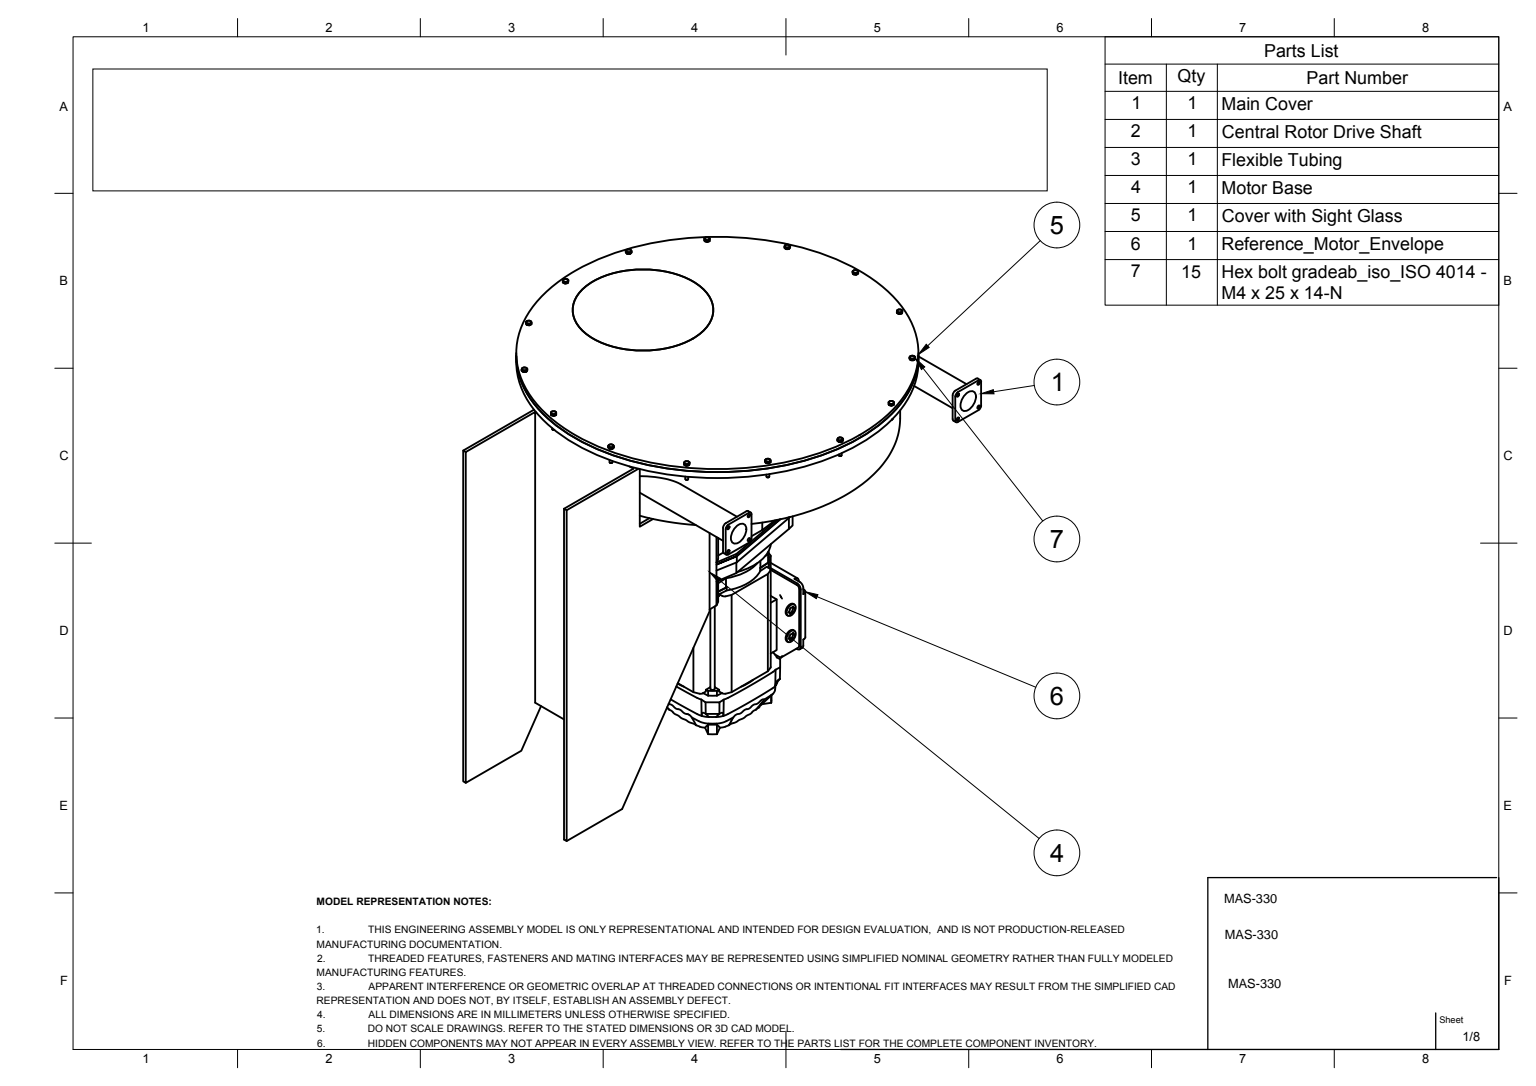
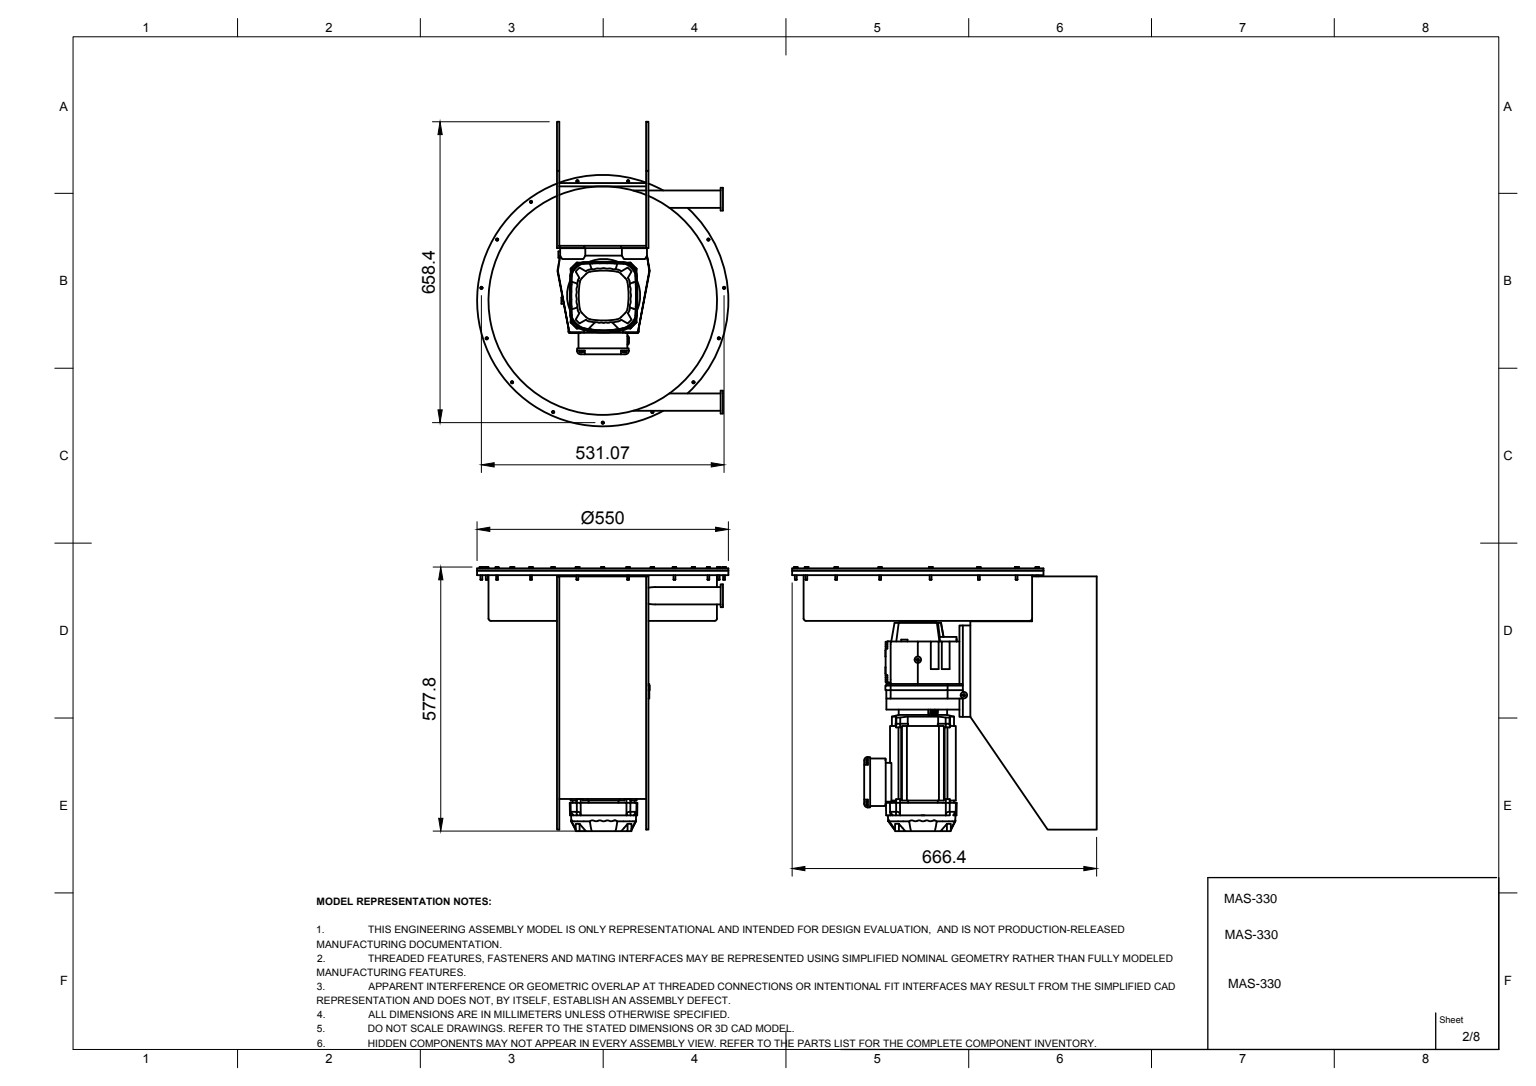
ISO-10303-21;
HEADER;
/* Generated by software containing ST-Developer
 * from STEP Tools, Inc. (www.steptools.com) 
 */

FILE_DESCRIPTION(
/* description */ ('STEP AP214'),
/* implementation_level */ '2;1');

FILE_NAME(
/* name */ 'MAS-330',
/* time_stamp */ '2026-10-12T14:05:15-07:00',
/* author */ (''),
/* organization */ (''),
/* preprocessor_version */ 'ST-DEVELOPER v20.2',
/* originating_system */ 'Autodesk Translation Framework v15.15.0.0',
/* authorisation */ '');

FILE_SCHEMA (('AUTOMOTIVE_DESIGN { 1 0 10303 214 3 1 1 }'));
ENDSEC;

DATA;
#10=MECHANICAL_DESIGN_GEOMETRIC_PRESENTATION_REPRESENTATION('',(#282,#283,
#284,#285,#286,#287,#288,#289),#39959);
#11=ITEM_DEFINED_TRANSFORMATION($,$,#18350,#19989);
#12=ITEM_DEFINED_TRANSFORMATION($,$,#18536,#19990);
#13=ITEM_DEFINED_TRANSFORMATION($,$,#18721,#19991);
#14=ITEM_DEFINED_TRANSFORMATION($,$,#18752,#19992);
#15=ITEM_DEFINED_TRANSFORMATION($,$,#18793,#19993);
#16=ITEM_DEFINED_TRANSFORMATION($,$,#18852,#19994);
#17=ITEM_DEFINED_TRANSFORMATION($,$,#19944,#19995);
#18=ITEM_DEFINED_TRANSFORMATION($,$,#19944,#19996);
#19=ITEM_DEFINED_TRANSFORMATION($,$,#19944,#19997);
#20=ITEM_DEFINED_TRANSFORMATION($,$,#19944,#19998);
#21=ITEM_DEFINED_TRANSFORMATION($,$,#19944,#19999);
#22=ITEM_DEFINED_TRANSFORMATION($,$,#19944,#20000);
#23=ITEM_DEFINED_TRANSFORMATION($,$,#19944,#20001);
#24=ITEM_DEFINED_TRANSFORMATION($,$,#19944,#20002);
#25=ITEM_DEFINED_TRANSFORMATION($,$,#19944,#20003);
#26=ITEM_DEFINED_TRANSFORMATION($,$,#19944,#20004);
#27=ITEM_DEFINED_TRANSFORMATION($,$,#19944,#20005);
#28=ITEM_DEFINED_TRANSFORMATION($,$,#19944,#20006);
#29=ITEM_DEFINED_TRANSFORMATION($,$,#19944,#20007);
#30=ITEM_DEFINED_TRANSFORMATION($,$,#19944,#20008);
#31=ITEM_DEFINED_TRANSFORMATION($,$,#19944,#20009);
#32=(
REPRESENTATION_RELATIONSHIP($,$,#40002,#40001)
REPRESENTATION_RELATIONSHIP_WITH_TRANSFORMATION(#11)
SHAPE_REPRESENTATION_RELATIONSHIP()
);
#33=(
REPRESENTATION_RELATIONSHIP($,$,#40003,#40001)
REPRESENTATION_RELATIONSHIP_WITH_TRANSFORMATION(#12)
SHAPE_REPRESENTATION_RELATIONSHIP()
);
#34=(
REPRESENTATION_RELATIONSHIP($,$,#40004,#40001)
REPRESENTATION_RELATIONSHIP_WITH_TRANSFORMATION(#13)
SHAPE_REPRESENTATION_RELATIONSHIP()
);
#35=(
REPRESENTATION_RELATIONSHIP($,$,#40005,#40001)
REPRESENTATION_RELATIONSHIP_WITH_TRANSFORMATION(#14)
SHAPE_REPRESENTATION_RELATIONSHIP()
);
#36=(
REPRESENTATION_RELATIONSHIP($,$,#40006,#40001)
REPRESENTATION_RELATIONSHIP_WITH_TRANSFORMATION(#15)
SHAPE_REPRESENTATION_RELATIONSHIP()
);
#37=(
REPRESENTATION_RELATIONSHIP($,$,#40007,#40001)
REPRESENTATION_RELATIONSHIP_WITH_TRANSFORMATION(#16)
SHAPE_REPRESENTATION_RELATIONSHIP()
);
#38=(
REPRESENTATION_RELATIONSHIP($,$,#40008,#40001)
REPRESENTATION_RELATIONSHIP_WITH_TRANSFORMATION(#17)
SHAPE_REPRESENTATION_RELATIONSHIP()
);
#39=(
REPRESENTATION_RELATIONSHIP($,$,#40008,#40001)
REPRESENTATION_RELATIONSHIP_WITH_TRANSFORMATION(#18)
SHAPE_REPRESENTATION_RELATIONSHIP()
);
#40=(
REPRESENTATION_RELATIONSHIP($,$,#40008,#40001)
REPRESENTATION_RELATIONSHIP_WITH_TRANSFORMATION(#19)
SHAPE_REPRESENTATION_RELATIONSHIP()
);
#41=(
REPRESENTATION_RELATIONSHIP($,$,#40008,#40001)
REPRESENTATION_RELATIONSHIP_WITH_TRANSFORMATION(#20)
SHAPE_REPRESENTATION_RELATIONSHIP()
);
#42=(
REPRESENTATION_RELATIONSHIP($,$,#40008,#40001)
REPRESENTATION_RELATIONSHIP_WITH_TRANSFORMATION(#21)
SHAPE_REPRESENTATION_RELATIONSHIP()
);
#43=(
REPRESENTATION_RELATIONSHIP($,$,#40008,#40001)
REPRESENTATION_RELATIONSHIP_WITH_TRANSFORMATION(#22)
SHAPE_REPRESENTATION_RELATIONSHIP()
);
#44=(
REPRESENTATION_RELATIONSHIP($,$,#40008,#40001)
REPRESENTATION_RELATIONSHIP_WITH_TRANSFORMATION(#23)
SHAPE_REPRESENTATION_RELATIONSHIP()
);
#45=(
REPRESENTATION_RELATIONSHIP($,$,#40008,#40001)
REPRESENTATION_RELATIONSHIP_WITH_TRANSFORMATION(#24)
SHAPE_REPRESENTATION_RELATIONSHIP()
);
#46=(
REPRESENTATION_RELATIONSHIP($,$,#40008,#40001)
REPRESENTATION_RELATIONSHIP_WITH_TRANSFORMATION(#25)
SHAPE_REPRESENTATION_RELATIONSHIP()
);
#47=(
REPRESENTATION_RELATIONSHIP($,$,#40008,#40001)
REPRESENTATION_RELATIONSHIP_WITH_TRANSFORMATION(#26)
SHAPE_REPRESENTATION_RELATIONSHIP()
);
#48=(
REPRESENTATION_RELATIONSHIP($,$,#40008,#40001)
REPRESENTATION_RELATIONSHIP_WITH_TRANSFORMATION(#27)
SHAPE_REPRESENTATION_RELATIONSHIP()
);
#49=(
REPRESENTATION_RELATIONSHIP($,$,#40008,#40001)
REPRESENTATION_RELATIONSHIP_WITH_TRANSFORMATION(#28)
SHAPE_REPRESENTATION_RELATIONSHIP()
);
#50=(
REPRESENTATION_RELATIONSHIP($,$,#40008,#40001)
REPRESENTATION_RELATIONSHIP_WITH_TRANSFORMATION(#29)
SHAPE_REPRESENTATION_RELATIONSHIP()
);
#51=(
REPRESENTATION_RELATIONSHIP($,$,#40008,#40001)
REPRESENTATION_RELATIONSHIP_WITH_TRANSFORMATION(#30)
SHAPE_REPRESENTATION_RELATIONSHIP()
);
#52=(
REPRESENTATION_RELATIONSHIP($,$,#40008,#40001)
REPRESENTATION_RELATIONSHIP_WITH_TRANSFORMATION(#31)
SHAPE_REPRESENTATION_RELATIONSHIP()
);
#53=CONTEXT_DEPENDENT_SHAPE_REPRESENTATION(#32,#39980);
#54=CONTEXT_DEPENDENT_SHAPE_REPRESENTATION(#33,#39981);
#55=CONTEXT_DEPENDENT_SHAPE_REPRESENTATION(#34,#39982);
#56=CONTEXT_DEPENDENT_SHAPE_REPRESENTATION(#35,#39983);
#57=CONTEXT_DEPENDENT_SHAPE_REPRESENTATION(#36,#39984);
#58=CONTEXT_DEPENDENT_SHAPE_REPRESENTATION(#37,#39985);
#59=CONTEXT_DEPENDENT_SHAPE_REPRESENTATION(#38,#39986);
#60=CONTEXT_DEPENDENT_SHAPE_REPRESENTATION(#39,#39987);
#61=CONTEXT_DEPENDENT_SHAPE_REPRESENTATION(#40,#39988);
#62=CONTEXT_DEPENDENT_SHAPE_REPRESENTATION(#41,#39989);
#63=CONTEXT_DEPENDENT_SHAPE_REPRESENTATION(#42,#39990);
#64=CONTEXT_DEPENDENT_SHAPE_REPRESENTATION(#43,#39991);
#65=CONTEXT_DEPENDENT_SHAPE_REPRESENTATION(#44,#39992);
#66=CONTEXT_DEPENDENT_SHAPE_REPRESENTATION(#45,#39993);
#67=CONTEXT_DEPENDENT_SHAPE_REPRESENTATION(#46,#39994);
#68=CONTEXT_DEPENDENT_SHAPE_REPRESENTATION(#47,#39995);
#69=CONTEXT_DEPENDENT_SHAPE_REPRESENTATION(#48,#39996);
#70=CONTEXT_DEPENDENT_SHAPE_REPRESENTATION(#49,#39997);
#71=CONTEXT_DEPENDENT_SHAPE_REPRESENTATION(#50,#39998);
#72=CONTEXT_DEPENDENT_SHAPE_REPRESENTATION(#51,#39999);
#73=CONTEXT_DEPENDENT_SHAPE_REPRESENTATION(#52,#40000);
#74=NEXT_ASSEMBLY_USAGE_OCCURRENCE('Main Cover:1','Main Cover:1',
'Main Cover:1',#40010,#40011,'Main Cover:1');
#75=NEXT_ASSEMBLY_USAGE_OCCURRENCE('Central Rotor Drive Shaft:1',
'Central Rotor Drive Shaft:1','Central Rotor Drive Shaft:1',#40010,#40012,
'Central Rotor Drive Shaft:1');
#76=NEXT_ASSEMBLY_USAGE_OCCURRENCE('Flexible Tubing:1',
'Flexible Tubing:1','Flexible Tubing:1',#40010,#40013,
'Flexible Tubing:1');
#77=NEXT_ASSEMBLY_USAGE_OCCURRENCE('Motor Base:1','Motor Base:1',
'Motor Base:1',#40010,#40014,'Motor Base:1');
#78=NEXT_ASSEMBLY_USAGE_OCCURRENCE('Cover with Sight Glass:1',
'Cover with Sight Glass:1','Cover with Sight Glass:1',#40010,#40015,
'Cover with Sight Glass:1');
#79=NEXT_ASSEMBLY_USAGE_OCCURRENCE('Reference_Motor_Envelope:1',
'Reference_Motor_Envelope:1','Reference_Motor_Envelope:1',#40010,#40016,
'Reference_Motor_Envelope:1');
#80=NEXT_ASSEMBLY_USAGE_OCCURRENCE(
'hex bolt gradeab_iso_ISO 4014 - M4 x 25 x 14-N:1',
'hex bolt gradeab_iso_ISO 4014 - M4 x 25 x 14-N:1',
'hex bolt gradeab_iso_ISO 4014 - M4 x 25 x 14-N:1',#40010,#40017,
'hex bolt gradeab_iso_ISO 4014 - M4 x 25 x 14-N:1');
#81=NEXT_ASSEMBLY_USAGE_OCCURRENCE(
'hex bolt gradeab_iso_ISO 4014 - M4 x 25 x 14-N:2',
'hex bolt gradeab_iso_ISO 4014 - M4 x 25 x 14-N:2',
'hex bolt gradeab_iso_ISO 4014 - M4 x 25 x 14-N:2',#40010,#40017,
'hex bolt gradeab_iso_ISO 4014 - M4 x 25 x 14-N:2');
#82=NEXT_ASSEMBLY_USAGE_OCCURRENCE(
'hex bolt gradeab_iso_ISO 4014 - M4 x 25 x 14-N:3',
'hex bolt gradeab_iso_ISO 4014 - M4 x 25 x 14-N:3',
'hex bolt gradeab_iso_ISO 4014 - M4 x 25 x 14-N:3',#40010,#40017,
'hex bolt gradeab_iso_ISO 4014 - M4 x 25 x 14-N:3');
#83=NEXT_ASSEMBLY_USAGE_OCCURRENCE(
'hex bolt gradeab_iso_ISO 4014 - M4 x 25 x 14-N:4',
'hex bolt gradeab_iso_ISO 4014 - M4 x 25 x 14-N:4',
'hex bolt gradeab_iso_ISO 4014 - M4 x 25 x 14-N:4',#40010,#40017,
'hex bolt gradeab_iso_ISO 4014 - M4 x 25 x 14-N:4');
#84=NEXT_ASSEMBLY_USAGE_OCCURRENCE(
'hex bolt gradeab_iso_ISO 4014 - M4 x 25 x 14-N:5',
'hex bolt gradeab_iso_ISO 4014 - M4 x 25 x 14-N:5',
'hex bolt gradeab_iso_ISO 4014 - M4 x 25 x 14-N:5',#40010,#40017,
'hex bolt gradeab_iso_ISO 4014 - M4 x 25 x 14-N:5');
#85=NEXT_ASSEMBLY_USAGE_OCCURRENCE(
'hex bolt gradeab_iso_ISO 4014 - M4 x 25 x 14-N:6',
'hex bolt gradeab_iso_ISO 4014 - M4 x 25 x 14-N:6',
'hex bolt gradeab_iso_ISO 4014 - M4 x 25 x 14-N:6',#40010,#40017,
'hex bolt gradeab_iso_ISO 4014 - M4 x 25 x 14-N:6');
#86=NEXT_ASSEMBLY_USAGE_OCCURRENCE(
'hex bolt gradeab_iso_ISO 4014 - M4 x 25 x 14-N:7',
'hex bolt gradeab_iso_ISO 4014 - M4 x 25 x 14-N:7',
'hex bolt gradeab_iso_ISO 4014 - M4 x 25 x 14-N:7',#40010,#40017,
'hex bolt gradeab_iso_ISO 4014 - M4 x 25 x 14-N:7');
#87=NEXT_ASSEMBLY_USAGE_OCCURRENCE(
'hex bolt gradeab_iso_ISO 4014 - M4 x 25 x 14-N:8',
'hex bolt gradeab_iso_ISO 4014 - M4 x 25 x 14-N:8',
'hex bolt gradeab_iso_ISO 4014 - M4 x 25 x 14-N:8',#40010,#40017,
'hex bolt gradeab_iso_ISO 4014 - M4 x 25 x 14-N:8');
#88=NEXT_ASSEMBLY_USAGE_OCCURRENCE(
'hex bolt gradeab_iso_ISO 4014 - M4 x 25 x 14-N:9',
'hex bolt gradeab_iso_ISO 4014 - M4 x 25 x 14-N:9',
'hex bolt gradeab_iso_ISO 4014 - M4 x 25 x 14-N:9',#40010,#40017,
'hex bolt gradeab_iso_ISO 4014 - M4 x 25 x 14-N:9');
#89=NEXT_ASSEMBLY_USAGE_OCCURRENCE(
'hex bolt gradeab_iso_ISO 4014 - M4 x 25 x 14-N:10',
'hex bolt gradeab_iso_ISO 4014 - M4 x 25 x 14-N:10',
'hex bolt gradeab_iso_ISO 4014 - M4 x 25 x 14-N:10',#40010,#40017,
'hex bolt gradeab_iso_ISO 4014 - M4 x 25 x 14-N:10');
#90=NEXT_ASSEMBLY_USAGE_OCCURRENCE(
'hex bolt gradeab_iso_ISO 4014 - M4 x 25 x 14-N:11',
'hex bolt gradeab_iso_ISO 4014 - M4 x 25 x 14-N:11',
'hex bolt gradeab_iso_ISO 4014 - M4 x 25 x 14-N:11',#40010,#40017,
'hex bolt gradeab_iso_ISO 4014 - M4 x 25 x 14-N:11');
#91=NEXT_ASSEMBLY_USAGE_OCCURRENCE(
'hex bolt gradeab_iso_ISO 4014 - M4 x 25 x 14-N:12',
'hex bolt gradeab_iso_ISO 4014 - M4 x 25 x 14-N:12',
'hex bolt gradeab_iso_ISO 4014 - M4 x 25 x 14-N:12',#40010,#40017,
'hex bolt gradeab_iso_ISO 4014 - M4 x 25 x 14-N:12');
#92=NEXT_ASSEMBLY_USAGE_OCCURRENCE(
'hex bolt gradeab_iso_ISO 4014 - M4 x 25 x 14-N:13',
'hex bolt gradeab_iso_ISO 4014 - M4 x 25 x 14-N:13',
'hex bolt gradeab_iso_ISO 4014 - M4 x 25 x 14-N:13',#40010,#40017,
'hex bolt gradeab_iso_ISO 4014 - M4 x 25 x 14-N:13');
#93=NEXT_ASSEMBLY_USAGE_OCCURRENCE(
'hex bolt gradeab_iso_ISO 4014 - M4 x 25 x 14-N:14',
'hex bolt gradeab_iso_ISO 4014 - M4 x 25 x 14-N:14',
'hex bolt gradeab_iso_ISO 4014 - M4 x 25 x 14-N:14',#40010,#40017,
'hex bolt gradeab_iso_ISO 4014 - M4 x 25 x 14-N:14');
#94=NEXT_ASSEMBLY_USAGE_OCCURRENCE(
'hex bolt gradeab_iso_ISO 4014 - M4 x 25 x 14-N:15',
'hex bolt gradeab_iso_ISO 4014 - M4 x 25 x 14-N:15',
'hex bolt gradeab_iso_ISO 4014 - M4 x 25 x 14-N:15',#40010,#40017,
'hex bolt gradeab_iso_ISO 4014 - M4 x 25 x 14-N:15');
#95=SPHERICAL_SURFACE('',#19264,20.3600000000001);
#96=SPHERICAL_SURFACE('',#19265,20.3600000000002);
#97=(
BOUNDED_CURVE()
B_SPLINE_CURVE(3,(#30732,#30733,#30734,#30735),.UNSPECIFIED.,.F.,.F.)
B_SPLINE_CURVE_WITH_KNOTS((4,4),(-1.,-3.7852598383457E-5),.UNSPECIFIED.)
CURVE()
GEOMETRIC_REPRESENTATION_ITEM()
RATIONAL_B_SPLINE_CURVE((1.,0.978516928803385,0.978516115613319,0.999997560429802))
REPRESENTATION_ITEM('')
);
#98=(
BOUNDED_CURVE()
B_SPLINE_CURVE(3,(#30762,#30763,#30764,#30765),.UNSPECIFIED.,.F.,.F.)
B_SPLINE_CURVE_WITH_KNOTS((4,4),(-1.,0.),.UNSPECIFIED.)
CURVE()
GEOMETRIC_REPRESENTATION_ITEM()
RATIONAL_B_SPLINE_CURVE((1.,0.998672257010864,0.998672257010864,1.))
REPRESENTATION_ITEM('')
);
#99=(
BOUNDED_CURVE()
B_SPLINE_CURVE(2,(#31270,#31271,#31272),.UNSPECIFIED.,.F.,.F.)
B_SPLINE_CURVE_WITH_KNOTS((3,3),(-7.67019091974518,-5.57466309126419),
 .UNSPECIFIED.)
CURVE()
GEOMETRIC_REPRESENTATION_ITEM()
RATIONAL_B_SPLINE_CURVE((1.51474535125471,1.4769886104751,1.42144161629559))
REPRESENTATION_ITEM('')
);
#100=(
BOUNDED_CURVE()
B_SPLINE_CURVE(2,(#31276,#31277,#31278),.UNSPECIFIED.,.F.,.F.)
B_SPLINE_CURVE_WITH_KNOTS((3,3),(-18.6605106590412,-16.5649828305604),
 .UNSPECIFIED.)
CURVE()
GEOMETRIC_REPRESENTATION_ITEM()
RATIONAL_B_SPLINE_CURVE((1.4214416162955,1.476988610475,1.51474535125461))
REPRESENTATION_ITEM('')
);
#101=(
BOUNDED_CURVE()
B_SPLINE_CURVE(2,(#31282,#31283,#31284),.UNSPECIFIED.,.F.,.F.)
B_SPLINE_CURVE_WITH_KNOTS((3,3),(-7.6701909197441,-5.57466309126325),
 .UNSPECIFIED.)
CURVE()
GEOMETRIC_REPRESENTATION_ITEM()
RATIONAL_B_SPLINE_CURVE((1.51474535125461,1.47698861047501,1.4214416162955))
REPRESENTATION_ITEM('')
);
#102=(
BOUNDED_CURVE()
B_SPLINE_CURVE(2,(#31288,#31289,#31290),.UNSPECIFIED.,.F.,.F.)
B_SPLINE_CURVE_WITH_KNOTS((3,3),(-18.660510659043,-16.564982830562),
 .UNSPECIFIED.)
CURVE()
GEOMETRIC_REPRESENTATION_ITEM()
RATIONAL_B_SPLINE_CURVE((1.42144161629558,1.47698861047509,1.5147453512547))
REPRESENTATION_ITEM('')
);
#103=(
BOUNDED_CURVE()
B_SPLINE_CURVE(2,(#31295,#31296,#31297),.UNSPECIFIED.,.F.,.F.)
B_SPLINE_CURVE_WITH_KNOTS((3,3),(0.289788647925159,0.47130189078059),
 .UNSPECIFIED.)
CURVE()
GEOMETRIC_REPRESENTATION_ITEM()
RATIONAL_B_SPLINE_CURVE((1.27594103621743,1.36080572125034,1.44372227312264))
REPRESENTATION_ITEM('')
);
#104=(
BOUNDED_CURVE()
B_SPLINE_CURVE(2,(#31299,#31300,#31301),.UNSPECIFIED.,.F.,.F.)
B_SPLINE_CURVE_WITH_KNOTS((3,3),(4.49748593074956,6.56746087072966),
 .UNSPECIFIED.)
CURVE()
GEOMETRIC_REPRESENTATION_ITEM()
RATIONAL_B_SPLINE_CURVE((1.14470058445899,1.15519608505713,1.14470058445899))
REPRESENTATION_ITEM('')
);
#105=(
BOUNDED_CURVE()
B_SPLINE_CURVE(2,(#31302,#31303,#31304),.UNSPECIFIED.,.F.,.F.)
B_SPLINE_CURVE_WITH_KNOTS((3,3),(0.289788647925165,0.4713018907806),
 .UNSPECIFIED.)
CURVE()
GEOMETRIC_REPRESENTATION_ITEM()
RATIONAL_B_SPLINE_CURVE((1.27594103621742,1.36080572125034,1.44372227312264))
REPRESENTATION_ITEM('')
);
#106=(
BOUNDED_CURVE()
B_SPLINE_CURVE(2,(#31308,#31309,#31310),.UNSPECIFIED.,.F.,.F.)
B_SPLINE_CURVE_WITH_KNOTS((3,3),(16.5649828305673,18.6605106590487),
 .UNSPECIFIED.)
CURVE()
GEOMETRIC_REPRESENTATION_ITEM()
RATIONAL_B_SPLINE_CURVE((1.514745351255,1.47698861047538,1.42144161629586))
REPRESENTATION_ITEM('')
);
#107=(
BOUNDED_CURVE()
B_SPLINE_CURVE(2,(#31314,#31315,#31316),.UNSPECIFIED.,.F.,.F.)
B_SPLINE_CURVE_WITH_KNOTS((3,3),(5.57466309126757,7.67019091974901),
 .UNSPECIFIED.)
CURVE()
GEOMETRIC_REPRESENTATION_ITEM()
RATIONAL_B_SPLINE_CURVE((1.4214416162959,1.47698861047542,1.51474535125504))
REPRESENTATION_ITEM('')
);
#108=(
BOUNDED_CURVE()
B_SPLINE_CURVE(2,(#31320,#31321,#31322),.UNSPECIFIED.,.F.,.F.)
B_SPLINE_CURVE_WITH_KNOTS((3,3),(16.5649828305679,18.6605106590493),
 .UNSPECIFIED.)
CURVE()
GEOMETRIC_REPRESENTATION_ITEM()
RATIONAL_B_SPLINE_CURVE((1.51474535125504,1.47698861047542,1.4214416162959))
REPRESENTATION_ITEM('')
);
#109=(
BOUNDED_CURVE()
B_SPLINE_CURVE(2,(#31325,#31326,#31327),.UNSPECIFIED.,.F.,.F.)
B_SPLINE_CURVE_WITH_KNOTS((3,3),(5.5746630912673,7.67019091974871),
 .UNSPECIFIED.)
CURVE()
GEOMETRIC_REPRESENTATION_ITEM()
RATIONAL_B_SPLINE_CURVE((1.42144161629587,1.47698861047539,1.514745351255))
REPRESENTATION_ITEM('')
);
#110=(
BOUNDED_CURVE()
B_SPLINE_CURVE(2,(#32616,#32617,#32618),.UNSPECIFIED.,.F.,.F.)
B_SPLINE_CURVE_WITH_KNOTS((3,3),(-33.3299544599618,-31.4526565385171),
 .UNSPECIFIED.)
CURVE()
GEOMETRIC_REPRESENTATION_ITEM()
RATIONAL_B_SPLINE_CURVE((1.20098306198357,1.20314118954088,1.20441859364838))
REPRESENTATION_ITEM('')
);
#111=(
BOUNDED_CURVE()
B_SPLINE_CURVE(3,(#32734,#32735,#32736,#32737),.UNSPECIFIED.,.F.,.F.)
B_SPLINE_CURVE_WITH_KNOTS((4,4),(0.,1.),.UNSPECIFIED.)
CURVE()
GEOMETRIC_REPRESENTATION_ITEM()
RATIONAL_B_SPLINE_CURVE((0.996955268533354,0.975234645152216,0.976249555641098,
1.))
REPRESENTATION_ITEM('')
);
#112=(
BOUNDED_CURVE()
B_SPLINE_CURVE(3,(#32739,#32740,#32741,#32742),.UNSPECIFIED.,.F.,.F.)
B_SPLINE_CURVE_WITH_KNOTS((4,4),(0.,1.),.UNSPECIFIED.)
CURVE()
GEOMETRIC_REPRESENTATION_ITEM()
RATIONAL_B_SPLINE_CURVE((1.,0.976245441159908,0.975234294192269,0.996966559097083))
REPRESENTATION_ITEM('')
);
#113=(
BOUNDED_CURVE()
B_SPLINE_CURVE(2,(#39863,#39864,#39865),.UNSPECIFIED.,.F.,.F.)
B_SPLINE_CURVE_WITH_KNOTS((3,3),(-0.935215532485105,-0.564489106699794),
 .UNSPECIFIED.)
CURVE()
GEOMETRIC_REPRESENTATION_ITEM()
RATIONAL_B_SPLINE_CURVE((1.84128182081917,1.84128182081917,1.70908373393142))
REPRESENTATION_ITEM('')
);
#114=(
BOUNDED_CURVE()
B_SPLINE_CURVE(2,(#39866,#39867,#39868),.UNSPECIFIED.,.F.,.F.)
B_SPLINE_CURVE_WITH_KNOTS((3,3),(-1.30594195827042,-0.935215532485105),
 .UNSPECIFIED.)
CURVE()
GEOMETRIC_REPRESENTATION_ITEM()
RATIONAL_B_SPLINE_CURVE((1.70908373393142,1.84128182081917,1.84128182081917))
REPRESENTATION_ITEM('')
);
#115=(
BOUNDED_CURVE()
B_SPLINE_CURVE(2,(#39871,#39872,#39873),.UNSPECIFIED.,.F.,.F.)
B_SPLINE_CURVE_WITH_KNOTS((3,3),(-0.935215532485106,-0.564489106699797),
 .UNSPECIFIED.)
CURVE()
GEOMETRIC_REPRESENTATION_ITEM()
RATIONAL_B_SPLINE_CURVE((1.84128182081917,1.84128182081917,1.70908373393142))
REPRESENTATION_ITEM('')
);
#116=(
BOUNDED_CURVE()
B_SPLINE_CURVE(2,(#39874,#39875,#39876),.UNSPECIFIED.,.F.,.F.)
B_SPLINE_CURVE_WITH_KNOTS((3,3),(-1.30594195827041,-0.935215532485105),
 .UNSPECIFIED.)
CURVE()
GEOMETRIC_REPRESENTATION_ITEM()
RATIONAL_B_SPLINE_CURVE((1.70908373393142,1.84128182081917,1.84128182081917))
REPRESENTATION_ITEM('')
);
#117=(
BOUNDED_CURVE()
B_SPLINE_CURVE(2,(#39879,#39880,#39881),.UNSPECIFIED.,.F.,.F.)
B_SPLINE_CURVE_WITH_KNOTS((3,3),(-1.30594195827042,-0.935215532485106),
 .UNSPECIFIED.)
CURVE()
GEOMETRIC_REPRESENTATION_ITEM()
RATIONAL_B_SPLINE_CURVE((1.70908373393142,1.84128182081917,1.84128182081917))
REPRESENTATION_ITEM('')
);
#118=(
BOUNDED_CURVE()
B_SPLINE_CURVE(2,(#39882,#39883,#39884),.UNSPECIFIED.,.F.,.F.)
B_SPLINE_CURVE_WITH_KNOTS((3,3),(-0.935215532485105,-0.564489106699797),
 .UNSPECIFIED.)
CURVE()
GEOMETRIC_REPRESENTATION_ITEM()
RATIONAL_B_SPLINE_CURVE((1.84128182081917,1.84128182081917,1.70908373393142))
REPRESENTATION_ITEM('')
);
#119=(
BOUNDED_CURVE()
B_SPLINE_CURVE(2,(#39887,#39888,#39889),.UNSPECIFIED.,.F.,.F.)
B_SPLINE_CURVE_WITH_KNOTS((3,3),(-1.30594195827042,-0.935215532485105),
 .UNSPECIFIED.)
CURVE()
GEOMETRIC_REPRESENTATION_ITEM()
RATIONAL_B_SPLINE_CURVE((1.70908373393142,1.84128182081917,1.84128182081917))
REPRESENTATION_ITEM('')
);
#120=(
BOUNDED_CURVE()
B_SPLINE_CURVE(2,(#39890,#39891,#39892),.UNSPECIFIED.,.F.,.F.)
B_SPLINE_CURVE_WITH_KNOTS((3,3),(-0.935215532485106,-0.564489106699794),
 .UNSPECIFIED.)
CURVE()
GEOMETRIC_REPRESENTATION_ITEM()
RATIONAL_B_SPLINE_CURVE((1.84128182081917,1.84128182081918,1.70908373393142))
REPRESENTATION_ITEM('')
);
#121=(
BOUNDED_CURVE()
B_SPLINE_CURVE(2,(#39895,#39896,#39897),.UNSPECIFIED.,.F.,.F.)
B_SPLINE_CURVE_WITH_KNOTS((3,3),(-0.935215532485105,-0.564489106699796),
 .UNSPECIFIED.)
CURVE()
GEOMETRIC_REPRESENTATION_ITEM()
RATIONAL_B_SPLINE_CURVE((1.84128182081917,1.84128182081917,1.70908373393142))
REPRESENTATION_ITEM('')
);
#122=(
BOUNDED_CURVE()
B_SPLINE_CURVE(2,(#39898,#39899,#39900),.UNSPECIFIED.,.F.,.F.)
B_SPLINE_CURVE_WITH_KNOTS((3,3),(-1.30594195827041,-0.935215532485106),
 .UNSPECIFIED.)
CURVE()
GEOMETRIC_REPRESENTATION_ITEM()
RATIONAL_B_SPLINE_CURVE((1.70908373393142,1.84128182081917,1.84128182081917))
REPRESENTATION_ITEM('')
);
#123=(
BOUNDED_CURVE()
B_SPLINE_CURVE(2,(#39903,#39904,#39905),.UNSPECIFIED.,.F.,.F.)
B_SPLINE_CURVE_WITH_KNOTS((3,3),(-1.3059419582704,-0.935215532485106),
 .UNSPECIFIED.)
CURVE()
GEOMETRIC_REPRESENTATION_ITEM()
RATIONAL_B_SPLINE_CURVE((1.70908373393143,1.84128182081917,1.84128182081918))
REPRESENTATION_ITEM('')
);
#124=(
BOUNDED_CURVE()
B_SPLINE_CURVE(2,(#39906,#39907,#39908),.UNSPECIFIED.,.F.,.F.)
B_SPLINE_CURVE_WITH_KNOTS((3,3),(-0.935215532485106,-0.564489106699775),
 .UNSPECIFIED.)
CURVE()
GEOMETRIC_REPRESENTATION_ITEM()
RATIONAL_B_SPLINE_CURVE((1.84128182081917,1.84128182081917,1.70908373393141))
REPRESENTATION_ITEM('')
);
#125=ORIENTED_CLOSED_SHELL('',*,#18265,.F.);
#126=ORIENTED_CLOSED_SHELL('',*,#18266,.F.);
#127=ORIENTED_CLOSED_SHELL('',*,#18267,.F.);
#128=ORIENTED_CLOSED_SHELL('',*,#18268,.F.);
#129=CONICAL_SURFACE('',#18879,28.6682517601201,1.23062314824616);
#130=CONICAL_SURFACE('',#18880,50.,0.475882249660419);
#131=CONICAL_SURFACE('',#18882,32.793965079916,0.986624506004945);
#132=CONICAL_SURFACE('',#18883,45.3097394023382,1.52321322351791);
#133=CONICAL_SURFACE('',#18886,0.857142857149273,0.197395559849881);
#134=CONICAL_SURFACE('',#18890,0.999999999925894,0.463647609000806);
#135=CONICAL_SURFACE('',#18893,0.499999999966139,0.463647608692697);
#136=CONICAL_SURFACE('',#18930,107.1412427187,0.174532925199605);
#137=CONICAL_SURFACE('',#18993,76.5,1.3264502315157);
#138=CONICAL_SURFACE('',#19016,6.99999999990287,0.785398163411024);
#139=CONICAL_SURFACE('',#19043,17.4625,0.785398163397448);
#140=CONICAL_SURFACE('',#19069,945.,0.0174532925199452);
#141=CONICAL_SURFACE('',#19072,6.75000000001091,0.785398163397448);
#142=CONICAL_SURFACE('',#19078,942.,0.0174532925199432);
#143=CONICAL_SURFACE('',#19090,6.34999999994079,0.785398163364011);
#144=CONICAL_SURFACE('',#19099,5.4999999998131,1.10714871774448);
#145=CONICAL_SURFACE('',#19291,96.9819619535671,1.14717901504738);
#146=CONICAL_SURFACE('',#19315,22.3000008196592,0.0174532925199444);
#147=CONICAL_SURFACE('',#19317,86.00000081803,0.0174532925199416);
#148=CONICAL_SURFACE('',#19319,22.3000010500621,0.0174532925199414);
#149=CONICAL_SURFACE('',#19321,942.000001054498,0.0174532925199525);
#150=CONICAL_SURFACE('',#19323,22.3000013536827,0.0174532925199416);
#151=CONICAL_SURFACE('',#19325,86.0000013640202,0.0174532925199415);
#152=CONICAL_SURFACE('',#19327,22.3000017511903,0.0174532925199381);
#153=CONICAL_SURFACE('',#19329,22.3000017511903,0.0174532925199378);
#154=CONICAL_SURFACE('',#19331,86.0000013640202,0.0174532925199428);
#155=CONICAL_SURFACE('',#19333,32.8000013531573,0.0174532925199434);
#156=CONICAL_SURFACE('',#19335,200.000000812291,0.0174532925199407);
#157=CONICAL_SURFACE('',#19337,32.8000008122913,0.0174532925199388);
#158=CONICAL_SURFACE('',#19339,86.0000008122913,0.0174532925199416);
#159=CONICAL_SURFACE('',#19341,22.3000008122913,0.0174532925199454);
#160=CONICAL_SURFACE('',#19343,941.999999061101,0.017453292519947);
#161=CONICAL_SURFACE('',#19389,25.2657032643209,0.0174532925199449);
#162=CONICAL_SURFACE('',#19394,25.2657032643207,0.0174532925199417);
#163=CONICAL_SURFACE('',#19396,945.,0.0174532925199452);
#164=CONICAL_SURFACE('',#19398,25.2657032643207,0.0174532925199417);
#165=CONICAL_SURFACE('',#19403,25.2657032643145,0.0174532925199406);
#166=CONICAL_SURFACE('',#19405,25.2657032643204,0.0174532925199395);
#167=CONICAL_SURFACE('',#19410,34.9999999991313,0.0174532925199434);
#168=CONICAL_SURFACE('',#19412,180.,0.017453292519941);
#169=CONICAL_SURFACE('',#19414,34.9999999991315,0.0174532925199386);
#170=CONICAL_SURFACE('',#19419,25.2657032643206,0.0174532925199426);
#171=CONICAL_SURFACE('',#19421,945.,0.0174532925199372);
#172=CONICAL_SURFACE('',#19904,107.1412427187,0.174532925199605);
#173=CONICAL_SURFACE('',#19906,107.1412427187,0.174532925199605);
#174=CONICAL_SURFACE('',#19908,107.1412427187,0.174532925199605);
#175=CONICAL_SURFACE('',#19910,107.1412427187,0.174532925199605);
#176=CONICAL_SURFACE('',#19958,1.61,0.785398163397443);
#177=CONICAL_SURFACE('',#19977,3.5,1.0471975511966);
#178=CONICAL_SURFACE('',#19978,3.5,1.0471975511966);
#179=CONICAL_SURFACE('',#19979,3.5,1.0471975511966);
#180=CONICAL_SURFACE('',#19980,3.5,1.0471975511966);
#181=CONICAL_SURFACE('',#19981,3.5,1.0471975511966);
#182=CONICAL_SURFACE('',#19982,3.5,1.0471975511966);
#183=BREP_WITH_VOIDS('Body1',#18269,(#125,#126,#127,#128));
#184=(
BOUNDED_SURFACE()
B_SPLINE_SURFACE(3,2,((#27814,#27815,#27816),(#27817,#27818,#27819),(#27820,
#27821,#27822),(#27823,#27824,#27825),(#27826,#27827,#27828),(#27829,#27830,
#27831),(#27832,#27833,#27834),(#27835,#27836,#27837),(#27838,#27839,#27840),
(#27841,#27842,#27843),(#27844,#27845,#27846),(#27847,#27848,#27849),(#27850,
#27851,#27852),(#27853,#27854,#27855),(#27856,#27857,#27858),(#27859,#27860,
#27861),(#27862,#27863,#27864),(#27865,#27866,#27867),(#27868,#27869,#27870),
(#27871,#27872,#27873),(#27874,#27875,#27876),(#27877,#27878,#27879),(#27880,
#27881,#27882),(#27883,#27884,#27885),(#27886,#27887,#27888),(#27889,#27890,
#27891),(#27892,#27893,#27894),(#27895,#27896,#27897),(#27898,#27899,#27900),
(#27901,#27902,#27903),(#27904,#27905,#27906),(#27907,#27908,#27909),(#27910,
#27911,#27912),(#27913,#27914,#27915),(#27916,#27917,#27918),(#27919,#27920,
#27921),(#27922,#27923,#27924),(#27925,#27926,#27927),(#27928,#27929,#27930),
(#27931,#27932,#27933),(#27934,#27935,#27936),(#27937,#27938,#27939),(#27940,
#27941,#27942),(#27943,#27944,#27945),(#27946,#27947,#27948),(#27949,#27950,
#27951),(#27952,#27953,#27954),(#27955,#27956,#27957),(#27958,#27959,#27960),
(#27961,#27962,#27963),(#27964,#27965,#27966),(#27967,#27968,#27969),(#27970,
#27971,#27972),(#27973,#27974,#27975),(#27976,#27977,#27978),(#27979,#27980,
#27981),(#27982,#27983,#27984),(#27985,#27986,#27987),(#27988,#27989,#27990),
(#27991,#27992,#27993),(#27994,#27995,#27996),(#27997,#27998,#27999),(#28000,
#28001,#28002),(#28003,#28004,#28005),(#28006,#28007,#28008),(#28009,#28010,
#28011),(#28012,#28013,#28014),(#28015,#28016,#28017),(#28018,#28019,#28020),
(#28021,#28022,#28023),(#28024,#28025,#28026),(#28027,#28028,#28029),(#28030,
#28031,#28032),(#28033,#28034,#28035),(#28036,#28037,#28038),(#28039,#28040,
#28041),(#28042,#28043,#28044),(#28045,#28046,#28047),(#28048,#28049,#28050),
(#28051,#28052,#28053),(#28054,#28055,#28056),(#28057,#28058,#28059),(#28060,
#28061,#28062),(#28063,#28064,#28065),(#28066,#28067,#28068),(#28069,#28070,
#28071),(#28072,#28073,#28074),(#28075,#28076,#28077),(#28078,#28079,#28080),
(#28081,#28082,#28083),(#28084,#28085,#28086),(#28087,#28088,#28089),(#28090,
#28091,#28092),(#28093,#28094,#28095),(#28096,#28097,#28098),(#28099,#28100,
#28101)),.UNSPECIFIED.,.F.,.F.,.F.)
B_SPLINE_SURFACE_WITH_KNOTS((4,2,2,2,2,2,2,2,2,2,2,2,2,2,2,2,2,2,2,2,2,
2,2,2,2,2,2,2,2,2,2,2,2,2,2,2,2,2,2,2,2,2,2,2,2,2,2,4),(3,3),(0.22178007142157,
0.223701231496081,0.225435349569694,0.227169467643307,0.228036526680114,
0.228903585716921,0.229770644753727,0.230204174272131,0.230637703790534,
0.231071233308937,0.231504762827341,0.231938292345744,0.232371821864147,
0.232805351382551,0.233238880900954,0.234105939937761,0.234972998974567,
0.235840058011374,0.237574176084987,0.239308294158601,0.241042412232214,
0.242776530305827,0.246244766453054,0.249713002600281,0.256649474894734,
0.260117711041961,0.263585947189187,0.270522419483641,0.277458891778094,
0.291331836367001,0.298268308661454,0.305204780955908,0.319077725544815,
0.332950670133721,0.346823614722628,0.353760087017082,0.360696559311535,
0.374569503900442,0.388442448489349,0.402315393078255,0.409251865372709,
0.416188337667162,0.423124809961615,0.430061282256069,0.433529518403295,
0.436997754550522,0.440465990697749,0.444121268845909),(-0.000187042000933031,
1.00006570533259),.UNSPECIFIED.)
GEOMETRIC_REPRESENTATION_ITEM()
RATIONAL_B_SPLINE_SURFACE(((1.00001671480553,0.955315105954543,1.00000587097346),
(1.00001553678529,0.958464392346589,1.00000545720104),(1.00001436299837,
0.961602361500747,1.00000504491554),(1.00001214511377,0.96753159221984,
1.00000426589711),(1.0000110971902,0.970333081805704,1.00000389782035),
(1.00000903364032,0.975849718381431,1.00000317301105),(1.00000802454064,
0.978547417281528,1.00000281857094),(1.00000657099102,0.982433296228171,
1.0000023080205),(1.0000060954059,0.98370471220148,1.00000214097413),(1.0000051861456,
0.986135503257278,1.000001821602),(1.00000475111726,0.987298495868281,1.00000166880095),
(1.00000393900491,0.989469574341258,1.00000138355144),(1.00000355798186,
0.990488190713896,1.00000124971942),(1.00000307531353,0.991778542734027,
1.00000108018511),(1.00000292909575,0.992169437270804,1.00000102882701),
(1.00000267340501,0.992852993744571,1.0000009390172),(1.00000256420741,
0.993144919550281,1.00000090066221),(1.00000239821197,0.993588687122249,
1.00000084235732),(1.00000234012324,0.993743979916236,1.00000082195401),
(1.00000227962719,0.993905708377709,1.00000080070514),(1.00000227804363,
0.993909941827738,1.00000080014892),(1.00000233322191,0.993762429746366,
1.00000081952996),(1.00000238907502,0.993613113593466,1.00000083914802),
(1.00000255214859,0.993177157271913,1.00000089642662),(1.00000265990449,
0.992889085671756,1.00000093427522),(1.00000291128676,0.992217047317989,
1.00000102257171),(1.00000305564197,0.991831132138118,1.0000010732756),
(1.00000337449658,0.990978715127399,1.00000118527134),(1.00000355003229,
0.990509442879127,1.00000124692718),(1.00000410591494,0.98902336174389,
1.00000144217757),(1.00000451382822,0.987932857764997,1.00000158545462),
(1.0000053771532,0.985624868901155,1.00000188869225),(1.00000583381796,
0.984404034076013,1.00000204909296),(1.00000677789068,0.981880176447102,
1.00000238069275),(1.00000726052111,0.980589925744053,1.00000255021374),
(1.00000873064634,0.976659734042192,1.00000306658626),(1.00000973994235,
0.973961510289341,1.00000342109532),(1.00001179196766,0.968475683150999,
1.00000414185669),(1.00001283513645,0.96568690486921,1.00000450826337),
(1.00001494361968,0.960050144712234,1.00000524885524),(1.00001601138312,
0.95719561576597,1.00000562390063),(1.00001814845983,0.951482414616923,
1.00000637453578),(1.00001921796653,0.948623225275015,1.00000675019349),
(1.00002242616289,0.940046522775516,1.00000787705289),(1.00002456438731,
0.934330253373406,1.00000862809117),(1.00002882929853,0.922928558871327,
1.00001012611521),(1.00003095610456,0.91724281507434,1.00001087314285),
(1.00003730979308,0.900257041725582,1.00001310483718),(1.00004150973089,
0.889029045332982,1.00001458003971),(1.00004772883642,0.872403062390114,
1.00001676446258),(1.00004978850184,0.866896810424999,1.00001748790749),
(1.00005387724354,0.855966082598523,1.00001892405307),(1.00005590801946,
0.850537063013456,1.00001963735072),(1.00006192256307,0.834457950174723,
1.00002174992247),(1.00006583638793,0.823994840153908,1.00002312462957),
(1.00007345352895,0.803631388209101,1.00002580010388),(1.00007715685939,
0.793731008091671,1.0000271008761),(1.00008791765573,0.764963395833388,
1.00003088054016),(1.00009462794849,0.747024286693254,1.00003323748955),
(1.00010382896234,0.722426553366422,1.00003646928952),(1.00010675138937,
0.71461381858396,1.00003749577419),(1.00011227304363,0.699852382375851,
1.00003943522156),(1.00011487430917,0.692898231787275,1.00004034890021),
(1.00012212392104,0.673517321968125,1.00004289528215),(1.00012616942783,
0.662702177158641,1.00004431624172),(1.0001325032316,0.645769563161906,
1.00004654095165),(1.00013478994257,0.639656333948816,1.00004734414493),
(1.0001374601242,0.632517944987879,1.00004828202993),(1.00013784258632,
0.631495481447842,1.00004841636742),(1.00013694003487,0.63390833726827,
1.00004809935173),(1.00013639387768,0.635368418638627,1.00004790751735),
(1.00013481186227,0.63959773443293,1.00004735184409),(1.00013378125052,
0.642352943082953,1.000046989848),(1.00013001435257,0.652423262814007,1.00004566674808),
(1.00012660145365,0.661547211425516,1.00004446798815),(1.00011821711893,
0.683961657570758,1.00004152304174),(1.00011324709426,0.697248382663264,
1.0000397773509),(1.00010199064016,0.727341072498234,1.00003582359008),
(1.00009570502111,0.744144870834123,1.00003361580473),(1.00008544083,0.771584872526209,
1.00003001057023),(1.00008187300066,0.781123007795138,1.00002875739195),
(1.000074536318,0.800736690215974,1.00002618042693),(1.00007076318398,0.810823681264022,
1.00002485513662),(1.000063033788,0.831487232491117,1.00002214023345),(1.0000590774879,
0.84206389463353,1.00002075060717),(1.00005100479812,0.863645197935074,
1.00001791512414),(1.00004688833189,0.874650043707415,1.0000164692405),
(1.00004060950573,0.891435682115803,1.00001426384112),(1.00003849870446,
0.897078639254129,1.00001352243505),(1.00003426394995,0.908399713630422,
1.00001203500336),(1.00003213787031,0.914083515546979,1.00001128823086),
(1.00002787459407,0.925480839114136,1.00000979078109),(1.00002573731916,
0.931194570120134,1.00000904007632),(1.00002134529738,0.94293607843551,
1.00000749740547),(1.00001909036436,0.94896435336469,1.000006705374),(1.00001684310806,
0.954972105552579,1.00000591603894)))
REPRESENTATION_ITEM('')
SURFACE()
);
#185=(
BOUNDED_SURFACE()
B_SPLINE_SURFACE(3,2,((#28385,#28386,#28387),(#28388,#28389,#28390),(#28391,
#28392,#28393),(#28394,#28395,#28396),(#28397,#28398,#28399),(#28400,#28401,
#28402),(#28403,#28404,#28405),(#28406,#28407,#28408),(#28409,#28410,#28411),
(#28412,#28413,#28414),(#28415,#28416,#28417),(#28418,#28419,#28420),(#28421,
#28422,#28423),(#28424,#28425,#28426),(#28427,#28428,#28429),(#28430,#28431,
#28432),(#28433,#28434,#28435),(#28436,#28437,#28438),(#28439,#28440,#28441),
(#28442,#28443,#28444),(#28445,#28446,#28447),(#28448,#28449,#28450),(#28451,
#28452,#28453),(#28454,#28455,#28456),(#28457,#28458,#28459),(#28460,#28461,
#28462),(#28463,#28464,#28465),(#28466,#28467,#28468),(#28469,#28470,#28471),
(#28472,#28473,#28474),(#28475,#28476,#28477),(#28478,#28479,#28480),(#28481,
#28482,#28483),(#28484,#28485,#28486),(#28487,#28488,#28489),(#28490,#28491,
#28492),(#28493,#28494,#28495),(#28496,#28497,#28498),(#28499,#28500,#28501),
(#28502,#28503,#28504),(#28505,#28506,#28507),(#28508,#28509,#28510),(#28511,
#28512,#28513),(#28514,#28515,#28516),(#28517,#28518,#28519),(#28520,#28521,
#28522),(#28523,#28524,#28525),(#28526,#28527,#28528),(#28529,#28530,#28531),
(#28532,#28533,#28534),(#28535,#28536,#28537),(#28538,#28539,#28540),(#28541,
#28542,#28543),(#28544,#28545,#28546),(#28547,#28548,#28549),(#28550,#28551,
#28552),(#28553,#28554,#28555),(#28556,#28557,#28558),(#28559,#28560,#28561),
(#28562,#28563,#28564),(#28565,#28566,#28567),(#28568,#28569,#28570),(#28571,
#28572,#28573),(#28574,#28575,#28576),(#28577,#28578,#28579),(#28580,#28581,
#28582),(#28583,#28584,#28585),(#28586,#28587,#28588),(#28589,#28590,#28591),
(#28592,#28593,#28594),(#28595,#28596,#28597),(#28598,#28599,#28600),(#28601,
#28602,#28603),(#28604,#28605,#28606),(#28607,#28608,#28609),(#28610,#28611,
#28612),(#28613,#28614,#28615),(#28616,#28617,#28618),(#28619,#28620,#28621),
(#28622,#28623,#28624),(#28625,#28626,#28627),(#28628,#28629,#28630),(#28631,
#28632,#28633),(#28634,#28635,#28636),(#28637,#28638,#28639),(#28640,#28641,
#28642),(#28643,#28644,#28645),(#28646,#28647,#28648),(#28649,#28650,#28651),
(#28652,#28653,#28654),(#28655,#28656,#28657),(#28658,#28659,#28660),(#28661,
#28662,#28663),(#28664,#28665,#28666),(#28667,#28668,#28669),(#28670,#28671,
#28672),(#28673,#28674,#28675),(#28676,#28677,#28678),(#28679,#28680,#28681),
(#28682,#28683,#28684),(#28685,#28686,#28687),(#28688,#28689,#28690)),
 .UNSPECIFIED.,.F.,.F.,.F.)
B_SPLINE_SURFACE_WITH_KNOTS((4,2,2,2,2,2,2,2,2,2,2,2,2,2,2,2,2,2,2,2,2,
2,2,2,2,2,2,2,2,2,2,2,2,2,2,2,2,2,2,2,2,2,2,2,2,2,2,2,2,2,4),(3,3),(0.,
0.00173411807361341,0.00346823614722682,0.00520235422084023,0.00606941325764693,
0.00693647229445363,0.00780353133126034,0.00867059036806704,0.00910411988647039,
0.00953764940487375,0.0099711789232771,0.0104047084416805,0.0108382379600838,
0.0112717674784872,0.0117052969968905,0.0121388265152939,0.0130058855521006,
0.0138729445889073,0.0156070626625207,0.0173411807361341,0.0190752988097475,
0.0208094168833609,0.0242776530305877,0.0277458891778145,0.0346823614722682,
0.038150597619495,0.0416188337667218,0.0485553060611754,0.0554917783556291,
0.0693647229445363,0.0832376675334436,0.0867059036806704,0.0901741398278972,
0.0971106121223509,0.110983556711258,0.124856501300165,0.131792973594619,
0.135261209741846,0.138729445889073,0.15260239047798,0.166475335066887,
0.180348279655794,0.183816515803021,0.187284751950248,0.194221224244702,
0.201157696539155,0.208094168833609,0.211562404980836,0.215030641128063,
0.218498877275289,0.222038288720656),(0.,1.00007117529817),
 .UNSPECIFIED.)
GEOMETRIC_REPRESENTATION_ITEM()
RATIONAL_B_SPLINE_SURFACE(((1.,0.954058032824739,1.00000653986642),(1.,
0.956926189621845,1.00000613158259),(1.,0.959774945923169,1.00000572606044),
(1.,0.965414443781637,1.00000492327455),(1.,0.968205662454782,1.00000452594291),
(1.,0.973699562224279,1.000003743883),(1.,0.976403365991766,1.00000335899492),
(1.,0.98034605056057,1.00000279775142),(1.,0.981641163134558,1.00000261339138),
(1.,0.984176833060148,1.00000225243725),(1.,0.985416251002957,1.00000207600537),
(1.,0.987758111159059,1.00000174264018),(1.,0.988874643995945,1.00000158370106),
(1.,0.99087726268354,1.0000012986271),(1.,0.991757284799027,1.00000117335542),
(1.,0.992797059568252,1.00000102534287),(1.,0.993098523876015,1.00000098242924),
(1.,0.993562924435804,1.00000091632155),(1.,0.993726976585977,1.00000089296862),
(1.,0.9939034030842,1.00000086785421),(1.,0.993913510674876,1.00000086641539),
(1.,0.993776600284822,1.00000088590466),(1.,0.993631545571422,1.00000090655329),
(1.,0.993199734841636,1.0000009680218),(1.,0.992914845213595,1.00000100857601),
(1.,0.99224575536465,1.00000110382135),(1.,0.991859782611137,1.0000011587648),
(1.,0.991003776450707,1.00000128061779),(1.,0.990532224611597,1.00000134774347),
(1.,0.989541347388611,1.00000148879544),(1.,0.98901957113283,1.0000015630706),
(1.,0.987391710342441,1.00000179479755),(1.,0.986223928377901,1.00000196103201),
(1.,0.983775371631144,1.00000230958552),(1.,0.982504716794789,1.000002490464),
(1.,0.97863152044244,1.00000304181581),(1.,0.975951927850889,1.00000342325741),
(1.,0.970485088654407,1.00000420146523),(1.,0.967696119306073,1.00000459847668),
(1.,0.962047336054619,1.00000540258435),(1.,0.959183960598246,1.00000581018755),
(1.,0.953462458079452,1.00000662464684),(1.,0.950596652764379,1.00000703259594),
(1.,0.941994603975872,1.00000825710271),(1.,0.936254194204132,1.00000907425347),
(1.,0.924794890941365,1.00001070549212),(1.,0.919075593477731,1.00001151963753),
(1.,0.901978842716718,1.00001395337019),(1.,0.890663248710558,1.00001556415175),
(1.,0.8738935874927,1.00001795132302),(1.,0.868330212597956,1.00001874327276),
(1.,0.857329904873204,1.00002030917312),(1.,0.851890471291245,1.00002108347973),
(1.,0.835762777169572,1.00002337926661),(1.,0.825264842647475,1.00002487365385),
(1.,0.804827719776929,1.00002778289048),(1.,0.794888487743137,1.00002919774608),
(1.,0.765999443480927,1.00003331011876),(1.,0.747972792915185,1.00003587622322),
(1.,0.714994849965956,1.00004057065307),(1.,0.700044230979255,1.00004269888259),
(1.,0.683764200151961,1.00004501635469),(1.,0.680628844586273,1.00004546267443),
(1.,0.674640520726457,1.0000463151159),(1.,0.671783516007252,1.00004672181222),
(1.,0.663635510374337,1.00004788168568),(1.,0.658767677401333,1.00004857462461),
(1.,0.645945349063695,1.0000503998907),(1.,0.639777818633445,1.00005127784233),
(1.,0.632581312956382,1.00005230226921),(1.,0.631555065114158,1.0000524483562),
(1.,0.63399275055746,1.00005210135022),(1.,0.635466148812585,1.0000518916111),
(1.,0.638664401233599,1.00005143633796),(1.,0.639895676582775,1.00005126106518),
(1.,0.642669442581869,1.00005086621794),(1.,0.644213120868507,1.00005064647441),
(1.,0.652691129180967,1.00004943962487),(1.,0.661906311274784,1.00004812783821),
(1.,0.684528677277457,1.00004490753092),(1.,0.697932027791846,1.00004299955598),
(1.,0.728267963131221,1.00003868121749),(1.,0.745198393491031,1.00003627116063),
(1.,0.768222924620666,1.0000329936049),(1.,0.772921247385803,1.00003232479585),
(1.,0.782497618983893,1.00003096159364),(1.,0.787373779802698,1.00003026746924),
(1.,0.802194699878368,1.00002815770243),(1.,0.812351834256105,1.00002671182829),
(1.,0.833145675250053,1.00002375181263),(1.,0.843782502229831,1.00002223765397),
(1.,0.86547121370724,1.00001915025295),(1.,0.876523345831396,1.00001757697535),
(1.,0.893367253742941,1.00001517923502),(1.,0.899026187982997,1.00001437368235),
(1.,0.910424400977938,1.00001275113994),(1.,0.916164825311843,1.00001193398711),
(1.,0.927638312474702,1.00001030072937),(1.,0.933380131170828,1.00000948337806),
(1.,0.944959178856698,1.00000783509371),(1.,0.950796193416408,1.00000700419121),
(1.,0.95659226878001,1.00000617911642)))
REPRESENTATION_ITEM('')
SURFACE()
);
#186=(
BOUNDED_SURFACE()
B_SPLINE_SURFACE(3,2,((#29356,#29357,#29358),(#29359,#29360,#29361),(#29362,
#29363,#29364),(#29365,#29366,#29367),(#29368,#29369,#29370),(#29371,#29372,
#29373),(#29374,#29375,#29376),(#29377,#29378,#29379),(#29380,#29381,#29382),
(#29383,#29384,#29385),(#29386,#29387,#29388),(#29389,#29390,#29391),(#29392,
#29393,#29394),(#29395,#29396,#29397),(#29398,#29399,#29400),(#29401,#29402,
#29403),(#29404,#29405,#29406),(#29407,#29408,#29409),(#29410,#29411,#29412),
(#29413,#29414,#29415),(#29416,#29417,#29418),(#29419,#29420,#29421),(#29422,
#29423,#29424),(#29425,#29426,#29427),(#29428,#29429,#29430),(#29431,#29432,
#29433),(#29434,#29435,#29436),(#29437,#29438,#29439),(#29440,#29441,#29442),
(#29443,#29444,#29445),(#29446,#29447,#29448),(#29449,#29450,#29451),(#29452,
#29453,#29454),(#29455,#29456,#29457),(#29458,#29459,#29460),(#29461,#29462,
#29463),(#29464,#29465,#29466),(#29467,#29468,#29469),(#29470,#29471,#29472),
(#29473,#29474,#29475),(#29476,#29477,#29478),(#29479,#29480,#29481),(#29482,
#29483,#29484),(#29485,#29486,#29487),(#29488,#29489,#29490),(#29491,#29492,
#29493),(#29494,#29495,#29496),(#29497,#29498,#29499),(#29500,#29501,#29502),
(#29503,#29504,#29505),(#29506,#29507,#29508),(#29509,#29510,#29511),(#29512,
#29513,#29514),(#29515,#29516,#29517),(#29518,#29519,#29520),(#29521,#29522,
#29523),(#29524,#29525,#29526),(#29527,#29528,#29529),(#29530,#29531,#29532),
(#29533,#29534,#29535),(#29536,#29537,#29538),(#29539,#29540,#29541),(#29542,
#29543,#29544),(#29545,#29546,#29547),(#29548,#29549,#29550),(#29551,#29552,
#29553),(#29554,#29555,#29556),(#29557,#29558,#29559),(#29560,#29561,#29562),
(#29563,#29564,#29565),(#29566,#29567,#29568),(#29569,#29570,#29571),(#29572,
#29573,#29574),(#29575,#29576,#29577),(#29578,#29579,#29580),(#29581,#29582,
#29583),(#29584,#29585,#29586),(#29587,#29588,#29589),(#29590,#29591,#29592),
(#29593,#29594,#29595),(#29596,#29597,#29598),(#29599,#29600,#29601),(#29602,
#29603,#29604),(#29605,#29606,#29607),(#29608,#29609,#29610),(#29611,#29612,
#29613),(#29614,#29615,#29616),(#29617,#29618,#29619),(#29620,#29621,#29622),
(#29623,#29624,#29625),(#29626,#29627,#29628),(#29629,#29630,#29631),(#29632,
#29633,#29634),(#29635,#29636,#29637),(#29638,#29639,#29640),(#29641,#29642,
#29643)),.UNSPECIFIED.,.F.,.F.,.F.)
B_SPLINE_SURFACE_WITH_KNOTS((4,2,2,2,2,2,2,2,2,2,2,2,2,2,2,2,2,2,2,2,2,
2,2,2,2,2,2,2,2,2,2,2,2,2,2,2,2,2,2,2,2,2,2,2,2,2,2,4),(3,3),(0.221817496371262,
0.223701231496101,0.225435349569714,0.227169467643327,0.228036526680134,
0.228903585716941,0.229770644753747,0.23020417427215,0.230637703790554,
0.231071233308957,0.23150476282736,0.231938292345764,0.232371821864167,
0.23280535138257,0.233238880900974,0.23410593993778,0.234972998974587,0.235840058011393,
0.237574176085006,0.23930829415862,0.241042412232233,0.242776530305846,
0.246244766453072,0.249713002600299,0.256649474894752,0.260117711041978,
0.263585947189204,0.270522419483657,0.27745889177811,0.291331836367015,
0.298268308661468,0.305204780955921,0.319077725544826,0.332950670133732,
0.346823614722637,0.35376008701709,0.360696559311543,0.374569503900448,
0.388442448489354,0.402315393078259,0.409251865372712,0.416188337667165,
0.423124809961617,0.43006128225607,0.433529518403296,0.436997754550523,
0.440465990697749,0.44408384389623),(-0.000149617051253964,1.00007479383841),
 .UNSPECIFIED.)
GEOMETRIC_REPRESENTATION_ITEM()
RATIONAL_B_SPLINE_SURFACE(((1.00001331480133,0.955500401761319,1.00000665559565),
(1.00001239101105,0.958587815164465,1.00000619382575),(1.00001147053421,
0.961664154694889,1.00000573371211),(1.0000097146529,0.967532512098177,
1.00000485600949),(1.00000887643813,0.970333922314243,1.00000443701574),
(1.00000722584258,0.975850402594055,1.00000361194172),(1.00000641868232,
0.978548025065446,1.00000320847102),(1.00000525601474,0.982433793918799,
1.00000262729484),(1.00000487560295,0.983705173871199,1.00000243714052),
(1.00000414830239,0.986135896059087,1.00000207358883),(1.00000380033123,
0.98729885572081,1.00000189965042),(1.00000315073751,0.989469872683854,
1.00000157494163),(1.00000284596418,0.990488460197697,1.00000142259628),
(1.00000245988668,0.991778775660097,1.00000122960987),(1.00000234292976,
0.992169659122265,1.00000117114726),(1.00000213840745,0.992853196229914,
1.00000106891383),(1.0000020510623,0.993145113764892,1.0000010252531),(1.0000019182856,
0.993588868764268,1.00000095888275),(1.0000018718215,0.993744157158601,
1.000000935657),(1.00000182343182,0.993905881037986,1.00000091146872),(1.00000182216515,
0.993910114368128,1.00000091083556),(1.00000186630125,0.993762606465926,
1.00000093289762),(1.00000191097712,0.993613294543411,1.0000009552295),
(1.00000204141667,0.993177350573097,1.00000102043159),(1.00000212760863,
0.992889287134443,1.00000106351589),(1.00000232868468,0.992217267820518,
1.00000116402665),(1.00000244415175,0.991831363574199,1.00000122174454),
(1.00000269919769,0.990978970713684,1.00000134923293),(1.00000283960547,
0.990509711760598,1.00000141941779),(1.00000328424576,0.989023672728241,
1.00000164167766),(1.00000361052809,0.987933199644816,1.00000180477459),
(1.00000430108584,0.985625276169944,1.00000214995985),(1.00000466636358,
0.984404475932691,1.0000023325492),(1.00000542150997,0.981880689808502,
1.00000271002002),(1.00000580755716,0.980590475660211,1.00000290299128),
(1.00000698348326,0.976660395306211,1.00000349079492),(1.00000779080056,
0.973962247998255,1.00000389434413),(1.00000943217783,0.968476576281456,
1.00000471481025),(1.00001026658934,0.965687877010012,1.00000513190289),
(1.00001195312625,0.960051276550606,1.00000597494271),(1.00001280721057,
0.957196828477568,1.00000640186909),(1.00001451661888,0.951483789191777,
1.00000725634151),(1.00001537209761,0.948624680855099,1.0000076839649),
(1.00001793827481,0.940048221346092,1.00000896670562),(1.00001964860115,
0.934332113895509,1.00000982163693),(1.00002306002512,0.922930742418279,
1.00001152688645),(1.0000247612181,0.917245159708875,1.00001237725232),
(1.00002984341657,0.900259867589174,1.00001491766259),(1.0000332028695,
0.889032189306294,1.00001659693363),(1.00003817741751,0.872406677399274,
1.00001908353327),(1.00003982490596,0.866900581435969,1.00001990705415),
(1.00004309541517,0.855970163292049,1.00002154186539),(1.00004471979543,
0.850541297518764,1.00002235383532),(1.00004953071814,0.834462640227989,
1.00002475864448),(1.00005266131459,0.823999826640663,1.00002632351831),
(1.00005875412544,0.803636951622608,1.00002936909777),(1.00006171635128,
0.79373685199774,1.00003084980912),(1.00007032371416,0.764970054768136,
1.00003515232371),(1.00007569115378,0.747031453875889,1.00003783531589),
(1.00008305087536,0.722434417430132,1.00004151417897),(1.00008538847094,
0.714621904001906,1.00004268265986),(1.00008980514053,0.699860885997467,
1.00004489039591),(1.00009188584494,0.692906932438445,1.00004593046605),
(1.00009768467601,0.673526571699192,1.00004882909547),(1.0001009206024,
0.662711733315835,1.00005044661999),(1.00010598689542,0.645779599024357,
1.0000529790797),(1.00010781599343,0.639666543011674,1.00005389338074),
(1.00010995182255,0.632528356305523,1.00005496100576),(1.00011025774696,
0.631505921714365,1.00005511392649),(1.00010953581267,0.633918709193333,
1.00005475305721),(1.00010909895159,0.635378749188762,1.0000545346859),
(1.00010783352659,0.639607945165404,1.00005390214494),(1.00010700915923,
0.642363075750804,1.00005349007302),(1.00010399608691,0.652433110183563,
1.00005198394532),(1.00010126617189,0.661556800302084,1.00005061935789),
(1.00009455969692,0.683970611397211,1.00004726702956),(1.00009058426569,
0.697256960064698,1.00004527985287),(1.0000815804353,0.727348797329703,
1.00004077915827),(1.00007655268435,0.744152119587061,1.00003826596438),
(1.00006834254686,0.77159134386594,1.00003416200863),(1.00006548870585,
0.781129208903971,1.00003273547501),(1.00005962022847,0.800742335641159,
1.00002980203187),(1.00005660216804,0.810829040908275,1.0000282934108),
(1.0000504195665,0.831492006708402,1.00002520294817),(1.00004725499489,
0.842068369196021,1.00002362109137),(1.00004079779896,0.863649061069833,
1.00002039336876),(1.00003750511341,0.874653595057445,1.00001874747236),
(1.00003248279597,0.891438757903646,1.00001623699448),(1.00003079440489,
0.897081555169982,1.00001539302783),(1.00002740710273,0.908402308800912,
1.00001369983595),(1.00002570649076,0.914085949687904,1.0000128497605),
(1.00002229637459,0.925482950352643,1.00001114516471),(1.00002058680775,
0.931196519480498,1.00001029061304),(1.00001709216721,0.942876010290598,
1.00000854376652),(1.00001530696519,0.948842360878052,1.00000765140752),
(1.00001352770684,0.954788847051718,1.00000676201955)))
REPRESENTATION_ITEM('')
SURFACE()
);
#187=(
BOUNDED_SURFACE()
B_SPLINE_SURFACE(3,2,((#30000,#30001,#30002),(#30003,#30004,#30005),(#30006,
#30007,#30008),(#30009,#30010,#30011),(#30012,#30013,#30014),(#30015,#30016,
#30017),(#30018,#30019,#30020),(#30021,#30022,#30023),(#30024,#30025,#30026),
(#30027,#30028,#30029),(#30030,#30031,#30032),(#30033,#30034,#30035),(#30036,
#30037,#30038),(#30039,#30040,#30041),(#30042,#30043,#30044),(#30045,#30046,
#30047),(#30048,#30049,#30050),(#30051,#30052,#30053),(#30054,#30055,#30056),
(#30057,#30058,#30059),(#30060,#30061,#30062),(#30063,#30064,#30065),(#30066,
#30067,#30068),(#30069,#30070,#30071),(#30072,#30073,#30074),(#30075,#30076,
#30077),(#30078,#30079,#30080),(#30081,#30082,#30083),(#30084,#30085,#30086),
(#30087,#30088,#30089),(#30090,#30091,#30092),(#30093,#30094,#30095),(#30096,
#30097,#30098),(#30099,#30100,#30101),(#30102,#30103,#30104),(#30105,#30106,
#30107),(#30108,#30109,#30110),(#30111,#30112,#30113),(#30114,#30115,#30116),
(#30117,#30118,#30119),(#30120,#30121,#30122),(#30123,#30124,#30125),(#30126,
#30127,#30128),(#30129,#30130,#30131),(#30132,#30133,#30134),(#30135,#30136,
#30137),(#30138,#30139,#30140),(#30141,#30142,#30143),(#30144,#30145,#30146),
(#30147,#30148,#30149),(#30150,#30151,#30152),(#30153,#30154,#30155),(#30156,
#30157,#30158),(#30159,#30160,#30161),(#30162,#30163,#30164),(#30165,#30166,
#30167),(#30168,#30169,#30170),(#30171,#30172,#30173),(#30174,#30175,#30176),
(#30177,#30178,#30179),(#30180,#30181,#30182),(#30183,#30184,#30185),(#30186,
#30187,#30188),(#30189,#30190,#30191),(#30192,#30193,#30194),(#30195,#30196,
#30197),(#30198,#30199,#30200),(#30201,#30202,#30203),(#30204,#30205,#30206),
(#30207,#30208,#30209),(#30210,#30211,#30212),(#30213,#30214,#30215),(#30216,
#30217,#30218),(#30219,#30220,#30221),(#30222,#30223,#30224),(#30225,#30226,
#30227),(#30228,#30229,#30230),(#30231,#30232,#30233),(#30234,#30235,#30236),
(#30237,#30238,#30239),(#30240,#30241,#30242),(#30243,#30244,#30245),(#30246,
#30247,#30248),(#30249,#30250,#30251),(#30252,#30253,#30254),(#30255,#30256,
#30257),(#30258,#30259,#30260),(#30261,#30262,#30263),(#30264,#30265,#30266),
(#30267,#30268,#30269),(#30270,#30271,#30272),(#30273,#30274,#30275),(#30276,
#30277,#30278),(#30279,#30280,#30281),(#30282,#30283,#30284),(#30285,#30286,
#30287),(#30288,#30289,#30290),(#30291,#30292,#30293),(#30294,#30295,#30296),
(#30297,#30298,#30299)),.UNSPECIFIED.,.F.,.F.,.F.)
B_SPLINE_SURFACE_WITH_KNOTS((4,2,2,2,2,2,2,2,2,2,2,2,2,2,2,2,2,2,2,2,2,
2,2,2,2,2,2,2,2,2,2,2,2,2,2,2,2,2,2,2,2,2,2,2,2,2,2,2,2,4),(3,3),(-0.000102234541641357,
0.00346823614722661,0.00520235422083992,0.00606941325764658,0.00693647229445323,
0.00780353133125988,0.00867059036806653,0.00910411988646986,0.00953764940487319,
0.00997117892327651,0.0104047084416798,0.0108382379600832,0.0112717674784865,
0.0117052969968898,0.0121388265152932,0.0130058855520998,0.0138729445889065,
0.0156070626625198,0.0173411807361331,0.0190752988097464,0.0208094168833597,
0.0242776530305863,0.0277458891778129,0.0346823614722661,0.0381505976194928,
0.0416188337667194,0.0485553060611726,0.0554917783556258,0.0693647229445323,
0.0832376675334387,0.0867059036806654,0.090174139827892,0.0971106121223452,
0.110983556711252,0.124856501300158,0.131792973594611,0.135261209741838,
0.138729445889065,0.152602390477971,0.166475335066877,0.180348279655784,
0.183816515803011,0.187284751950237,0.19422122424469,0.201157696539144,
0.208094168833597,0.211562404980823,0.21503064112805,0.218498877275277,
0.22202653747512),(0.,1.00010223454164),.UNSPECIFIED.)
GEOMETRIC_REPRESENTATION_ITEM()
RATIONAL_B_SPLINE_SURFACE(((1.,0.953549407570009,1.00000949771005),(1.,
0.959455865791245,1.00000829002195),(1.,0.965295688977991,1.00000709595866),
(1.,0.973698745410201,1.00000537779342),(1.,0.976402633150356,1.00000482493197),
(1.,0.980345440167197,1.00000401874983),(1.,0.981640592963782,1.00000375393113),
(1.,0.9841763416393,1.00000323544892),(1.,0.985415798074981,1.0000029820184),
(1.,0.987757730962312,1.00000250316553),(1.,0.988874298475363,1.00000227486199),
(1.,0.990876979358417,1.00000186537567),(1.,0.991757028804683,1.00000168543276),
(1.,0.992796835866325,1.00000147282437),(1.,0.993098309536668,1.00000141118232),
(1.,0.99356272451931,1.00000131622382),(1.,0.993726781764482,1.00000128267918),
(1.,0.993903213741988,1.0000012466043),(1.,0.993913321646593,1.00000124453754),
(1.,0.993776407004476,1.00000127253235),(1.,0.993631347786124,1.00000130219248),
(1.,0.993199523645578,1.00000139048717),(1.,0.992914625169687,1.0000014487401),
(1.,0.992245514540845,1.00000158555253),(1.,0.99185952980013,1.00000166447448),
(1.,0.991003497054706,1.00000183950671),(1.,0.990531930570611,1.00000193592748),
(1.,0.989541022573869,1.00000213853753),(1.,0.989019230113308,1.00000224522795),
(1.,0.987391318766343,1.00000257808549),(1.,0.986223500534092,1.00000281686822),
(1.,0.983774867742231,1.00000331753792),(1.,0.982504173443108,1.00000357735562),
(1.,0.978630856801064,1.00000436932912),(1.,0.975951180989188,1.00000491723998),
(1.,0.970484172008772,1.00000603507429),(1.,0.96769511604352,1.00000660535001),
(1.,0.96204615735736,1.00000776038741),(1.,0.959182692973428,1.00000834587735),
(1.,0.953461012761225,1.00000951578406),(1.,0.950595118442744,1.00001010177084),
(1.,0.941992802500896,1.0000118606785),(1.,0.936252214448483,1.00001303445127),
(1.,0.924792555293885,1.00001537759728),(1.,0.919073080205329,1.0000165470531),
(1.,0.901975798471311,1.00002004291863),(1.,0.890659853037534,1.00002235667962),
(1.,0.873889671000668,1.00002578566336),(1.,0.868326123324781,1.00002692323686),
(1.,0.857325473963624,1.00002917252955),(1.,0.851885871450147,1.00003028476009),
(1.,0.83575767644592,1.00003358247733),(1.,0.825259415892199,1.00003572904704),
(1.,0.804821658304747,1.0000399079366),(1.,0.794882117587898,1.00004194026538),
(1.,0.765992176118451,1.00004784736523),(1.,0.74796496570046,1.00005153337242),
(1.,0.714985998549083,1.0000582765516),(1.,0.700034915249734,1.0000613335859),
(1.,0.683754378804637,1.00006466245226),(1.,0.680618925863469,1.00006530355545),
(1.,0.674630416028701,1.00006652802056),(1.,0.671773322578567,1.00006711220784),
(1.,0.663625063888358,1.00006877827483),(1.,0.658757079736063,1.00006977362708),
(1.,0.645934353180302,1.00007239547823),(1.,0.63976663119061,1.00007365658669),
(1.,0.632569902032773,1.0000751280953),(1.,0.631543622312258,1.00007533793778),
(1.,0.633981383455941,1.00007483949099),(1.,0.63545482746786,1.00007453821724),
(1.,0.638653179224426,1.00007388425319),(1.,0.639884492811753,1.00007363248763),
(1.,0.642658344954122,1.00007306532063),(1.,0.644202071179115,1.00007274967634),
(1.,0.652680342816058,1.00007101613191),(1.,0.661895811073965,1.00006913185356),
(1.,0.684518879688121,1.00006450613546),(1.,0.697922646449475,1.00006176547956),
(1.,0.728259523947718,1.00005556252603),(1.,0.745190480114726,1.00005210066894),
(1.,0.768215726310939,1.00004739271796),(1.,0.772914194992678,1.00004643202638),
(1.,0.782490864005998,1.00004447389364),(1.,0.787367176263245,1.00004347683855),
(1.,0.802188556632332,1.00004044632449),(1.,0.81234600646155,1.00003836944003),
(1.,0.833140493248966,1.00003411761038),(1.,0.843777650575237,1.00003194264058),
(1.,0.865467035644792,1.00002750783189),(1.,0.876519511015255,1.00002524794239),
(1.,0.893363942044945,1.00002180377701),(1.,0.899023052036312,1.00002064666398),
(1.,0.910421619025157,1.00001831600944),(1.,0.916162221641087,1.00001714223369),
(1.,0.927636065134229,1.00001479618742),(1.,0.933378062154726,1.00001362212656),
(1.,0.944938051744135,1.00001125846608),(1.,0.950755904868764,1.00001006889499),
(1.,0.956533186645504,1.00000888761948)))
REPRESENTATION_ITEM('')
SURFACE()
);
#188=(
BOUNDED_SURFACE()
B_SPLINE_SURFACE(3,1,((#30722,#30723),(#30724,#30725),(#30726,#30727),(#30728,
#30729)),.UNSPECIFIED.,.F.,.F.,.F.)
B_SPLINE_SURFACE_WITH_KNOTS((4,4),(2,2),(0.,1.),(0.,1.),.UNSPECIFIED.)
GEOMETRIC_REPRESENTATION_ITEM()
RATIONAL_B_SPLINE_SURFACE(((1.,1.),(0.978516115582536,0.975189339715083),
(0.978516115582536,0.975189339715083),(1.,1.)))
REPRESENTATION_ITEM('')
SURFACE()
);
#189=(
BOUNDED_SURFACE()
B_SPLINE_SURFACE(3,1,((#30753,#30754),(#30755,#30756),(#30757,#30758),(#30759,
#30760)),.UNSPECIFIED.,.F.,.F.,.F.)
B_SPLINE_SURFACE_WITH_KNOTS((4,4),(2,2),(0.,1.),(0.,0.740226077012362),
 .UNSPECIFIED.)
GEOMETRIC_REPRESENTATION_ITEM()
RATIONAL_B_SPLINE_SURFACE(((1.,1.),(0.998672257010864,0.999507458473034),
(0.998672257010864,0.999507458473034),(1.,1.)))
REPRESENTATION_ITEM('')
SURFACE()
);
#190=(
BOUNDED_SURFACE()
B_SPLINE_SURFACE(3,1,((#31681,#31682),(#31683,#31684),(#31685,#31686),(#31687,
#31688)),.UNSPECIFIED.,.F.,.F.,.F.)
B_SPLINE_SURFACE_WITH_KNOTS((4,4),(2,2),(0.,1.),(-0.000822310060064629,
0.),.UNSPECIFIED.)
GEOMETRIC_REPRESENTATION_ITEM()
RATIONAL_B_SPLINE_SURFACE(((1.,1.),(0.962057791684876,0.962057791684876),
(0.962057791684876,0.962057791684876),(1.,1.)))
REPRESENTATION_ITEM('')
SURFACE()
);
#191=(
BOUNDED_SURFACE()
B_SPLINE_SURFACE(3,1,((#31700,#31701),(#31702,#31703),(#31704,#31705),(#31706,
#31707)),.UNSPECIFIED.,.F.,.F.,.F.)
B_SPLINE_SURFACE_WITH_KNOTS((4,4),(2,2),(0.,1.),(-0.000910780085741153,
0.),.UNSPECIFIED.)
GEOMETRIC_REPRESENTATION_ITEM()
RATIONAL_B_SPLINE_SURFACE(((1.,1.),(0.962057791684877,0.962057791684877),
(0.962057791684877,0.962057791684877),(1.,1.)))
REPRESENTATION_ITEM('')
SURFACE()
);
#192=(
BOUNDED_SURFACE()
B_SPLINE_SURFACE(3,1,((#31721,#31722),(#31723,#31724),(#31725,#31726),(#31727,
#31728)),.UNSPECIFIED.,.F.,.F.,.F.)
B_SPLINE_SURFACE_WITH_KNOTS((4,4),(2,2),(0.,1.),(0.,1.),.UNSPECIFIED.)
GEOMETRIC_REPRESENTATION_ITEM()
RATIONAL_B_SPLINE_SURFACE(((1.,1.),(0.962057791684877,0.975189339715083),
(0.962057791684877,0.975189339715083),(1.,1.)))
REPRESENTATION_ITEM('')
SURFACE()
);
#193=(
BOUNDED_SURFACE()
B_SPLINE_SURFACE(3,1,((#31772,#31773,#31774),(#31775,#31776,#31777),(#31778,
#31779,#31780),(#31781,#31782,#31783)),.UNSPECIFIED.,.F.,.F.,.F.)
B_SPLINE_SURFACE_WITH_KNOTS((4,4),(2,1,2),(0.633064943864098,0.634076354292062),
(-0.000184246289843766,0.,1.),.UNSPECIFIED.)
GEOMETRIC_REPRESENTATION_ITEM()
RATIONAL_B_SPLINE_SURFACE(((0.791557642220831,0.791557642220831,0.816814678743125),
(0.791557642220831,0.791557642220831,0.816814678743125),(0.791557642220831,
0.791557642220831,0.816814678743125),(0.791557642220831,0.791557642220831,
0.816814678743125)))
REPRESENTATION_ITEM('')
SURFACE()
);
#194=(
BOUNDED_SURFACE()
B_SPLINE_SURFACE(3,1,((#31793,#31794),(#31795,#31796),(#31797,#31798),(#31799,
#31800)),.UNSPECIFIED.,.F.,.F.,.F.)
B_SPLINE_SURFACE_WITH_KNOTS((4,4),(2,2),(0.,0.365923647633872),(0.,1.),
 .UNSPECIFIED.)
GEOMETRIC_REPRESENTATION_ITEM()
RATIONAL_B_SPLINE_SURFACE(((1.,1.),(0.89042205119026,0.903699651216535),
(0.820941265109217,0.84263787732833),(0.791557641756873,0.816814678335385)))
REPRESENTATION_ITEM('')
SURFACE()
);
#195=(
BOUNDED_SURFACE()
B_SPLINE_SURFACE(3,1,((#31831,#31832),(#31833,#31834),(#31835,#31836),(#31837,
#31838)),.UNSPECIFIED.,.F.,.F.,.F.)
B_SPLINE_SURFACE_WITH_KNOTS((4,4),(2,2),(0.,1.),(-0.000981925268428012,
0.),.UNSPECIFIED.)
GEOMETRIC_REPRESENTATION_ITEM()
RATIONAL_B_SPLINE_SURFACE(((1.,1.),(0.96205779168488,0.96205779168488),
(0.96205779168488,0.96205779168488),(1.,1.)))
REPRESENTATION_ITEM('')
SURFACE()
);
#196=(
BOUNDED_SURFACE()
B_SPLINE_SURFACE(3,1,((#31853,#31854),(#31855,#31856),(#31857,#31858),(#31859,
#31860)),.UNSPECIFIED.,.F.,.F.,.F.)
B_SPLINE_SURFACE_WITH_KNOTS((4,4),(2,2),(0.,1.),(0.,1.),.UNSPECIFIED.)
GEOMETRIC_REPRESENTATION_ITEM()
RATIONAL_B_SPLINE_SURFACE(((1.,1.),(0.96205779168488,0.975189339715083),
(0.96205779168488,0.975189339715083),(1.,1.)))
REPRESENTATION_ITEM('')
SURFACE()
);
#197=(
BOUNDED_SURFACE()
B_SPLINE_SURFACE(3,1,((#31906,#31907),(#31908,#31909),(#31910,#31911),(#31912,
#31913)),.UNSPECIFIED.,.F.,.F.,.F.)
B_SPLINE_SURFACE_WITH_KNOTS((4,4),(2,2),(0.,1.),(-0.000863309921543448,
0.),.UNSPECIFIED.)
GEOMETRIC_REPRESENTATION_ITEM()
RATIONAL_B_SPLINE_SURFACE(((1.,1.),(0.96207291357299,0.96207291357299),
(0.96207291357299,0.96207291357299),(1.,1.)))
REPRESENTATION_ITEM('')
SURFACE()
);
#198=(
BOUNDED_SURFACE()
B_SPLINE_SURFACE(3,1,((#31927,#31928),(#31929,#31930),(#31931,#31932),(#31933,
#31934)),.UNSPECIFIED.,.F.,.F.,.F.)
B_SPLINE_SURFACE_WITH_KNOTS((4,4),(2,2),(0.,1.),(0.,1.),.UNSPECIFIED.)
GEOMETRIC_REPRESENTATION_ITEM()
RATIONAL_B_SPLINE_SURFACE(((1.,1.),(0.96207291357299,0.975189339715083),
(0.96207291357299,0.975189339715083),(1.,1.)))
REPRESENTATION_ITEM('')
SURFACE()
);
#199=(
BOUNDED_SURFACE()
B_SPLINE_SURFACE(3,1,((#31980,#31981),(#31982,#31983),(#31984,#31985),(#31986,
#31987)),.UNSPECIFIED.,.F.,.F.,.F.)
B_SPLINE_SURFACE_WITH_KNOTS((4,4),(2,2),(0.,1.),(-0.000880114866331669,
0.),.UNSPECIFIED.)
GEOMETRIC_REPRESENTATION_ITEM()
RATIONAL_B_SPLINE_SURFACE(((1.,1.),(0.962072913572991,0.962072913572991),
(0.962072913572991,0.962072913572991),(1.,1.)))
REPRESENTATION_ITEM('')
SURFACE()
);
#200=(
BOUNDED_SURFACE()
B_SPLINE_SURFACE(3,1,((#32001,#32002),(#32003,#32004),(#32005,#32006),(#32007,
#32008)),.UNSPECIFIED.,.F.,.F.,.F.)
B_SPLINE_SURFACE_WITH_KNOTS((4,4),(2,2),(0.,1.),(-0.000751572727532702,
0.),.UNSPECIFIED.)
GEOMETRIC_REPRESENTATION_ITEM()
RATIONAL_B_SPLINE_SURFACE(((1.,1.),(0.962057791684879,0.962057791684879),
(0.962057791684879,0.962057791684879),(1.,1.)))
REPRESENTATION_ITEM('')
SURFACE()
);
#201=(
BOUNDED_SURFACE()
B_SPLINE_SURFACE(3,1,((#32916,#32917),(#32918,#32919),(#32920,#32921),(#32922,
#32923)),.UNSPECIFIED.,.F.,.F.,.F.)
B_SPLINE_SURFACE_WITH_KNOTS((4,4),(2,2),(0.,1.),(0.,1.),.UNSPECIFIED.)
GEOMETRIC_REPRESENTATION_ITEM()
RATIONAL_B_SPLINE_SURFACE(((1.,1.),(0.962057791684879,0.975189339715082),
(0.962057791684879,0.975189339715082),(1.,1.)))
REPRESENTATION_ITEM('')
SURFACE()
);
#202=(
BOUNDED_SURFACE()
B_SPLINE_SURFACE(3,1,((#32926,#32927,#32928,#32929),(#32930,#32931,#32932,
#32933),(#32934,#32935,#32936,#32937),(#32938,#32939,#32940,#32941),(#32942,
#32943,#32944,#32945),(#32946,#32947,#32948,#32949),(#32950,#32951,#32952,
#32953),(#32954,#32955,#32956,#32957),(#32958,#32959,#32960,#32961),(#32962,
#32963,#32964,#32965)),.UNSPECIFIED.,.F.,.F.,.F.)
B_SPLINE_SURFACE_WITH_KNOTS((4,3,3,4),(2,1,1,2),(-0.000662388520973799,
0.,1.,1.00066238358002),(-0.00076018000588443,0.,0.676109671237994,0.676144257435705),
 .UNSPECIFIED.)
GEOMETRIC_REPRESENTATION_ITEM()
RATIONAL_B_SPLINE_SURFACE(((1.,1.,1.,1.),(1.,1.,1.,1.),(1.,1.,1.,1.),(1.,
1.,1.,1.),(0.998736553042339,0.998736553042339,0.999455940415833,0.999455940415833),
(0.998736553042339,0.998736553042339,0.999455940415833,0.999455940415833),
(1.,1.,1.,1.),(1.,1.,1.,1.),(1.,1.,1.,1.),(1.,1.,1.,1.)))
REPRESENTATION_ITEM('')
SURFACE()
);
#203=(
BOUNDED_SURFACE()
B_SPLINE_SURFACE(3,1,((#32993,#32994),(#32995,#32996),(#32997,#32998),(#32999,
#33000)),.UNSPECIFIED.,.F.,.F.,.F.)
B_SPLINE_SURFACE_WITH_KNOTS((4,4),(2,2),(0.,1.),(0.,1.),.UNSPECIFIED.)
GEOMETRIC_REPRESENTATION_ITEM()
RATIONAL_B_SPLINE_SURFACE(((1.,1.),(0.962072913572991,0.975189339715083),
(0.962072913572991,0.975189339715083),(1.,1.)))
REPRESENTATION_ITEM('')
SURFACE()
);
#204=(
BOUNDED_SURFACE()
B_SPLINE_SURFACE(3,1,((#33002,#33003,#33004,#33005),(#33006,#33007,#33008,
#33009),(#33010,#33011,#33012,#33013),(#33014,#33015,#33016,#33017)),
 .UNSPECIFIED.,.F.,.F.,.F.)
B_SPLINE_SURFACE_WITH_KNOTS((4,4),(2,1,1,2),(0.847974360952231,1.),(-0.000384803530329693,
0.,1.,1.001),.UNSPECIFIED.)
GEOMETRIC_REPRESENTATION_ITEM()
RATIONAL_B_SPLINE_SURFACE(((0.9997286731407,0.9997286731407,0.99414139959028,
0.99414139959028),(0.999802900849163,0.999802900849163,0.995744154600748,
0.995744154600748),(0.999893343135597,0.999893343135597,0.997697021403988,
0.997697021403988),(1.,1.,1.,1.)))
REPRESENTATION_ITEM('')
SURFACE()
);
#205=(
BOUNDED_SURFACE()
B_SPLINE_SURFACE(3,1,((#33043,#33044),(#33045,#33046),(#33047,#33048),(#33049,
#33050)),.UNSPECIFIED.,.F.,.F.,.F.)
B_SPLINE_SURFACE_WITH_KNOTS((4,4),(2,2),(0.,0.366201644461032),(0.,1.),
 .UNSPECIFIED.)
GEOMETRIC_REPRESENTATION_ITEM()
RATIONAL_B_SPLINE_SURFACE(((1.,1.),(0.890338803435454,0.903626490622545),
(0.820835717386409,0.842545118861594),(0.791490741852866,0.816755884717148)))
REPRESENTATION_ITEM('')
SURFACE()
);
#206=(
BOUNDED_SURFACE()
B_SPLINE_SURFACE(3,1,((#33065,#33066),(#33067,#33068),(#33069,#33070),(#33071,
#33072)),.UNSPECIFIED.,.F.,.F.,.F.)
B_SPLINE_SURFACE_WITH_KNOTS((4,4),(2,2),(0.,1.),(0.,0.966511290545803),
 .UNSPECIFIED.)
GEOMETRIC_REPRESENTATION_ITEM()
RATIONAL_B_SPLINE_SURFACE(((1.,1.),(0.969175395688119,0.979164837438946),
(0.969175395688119,0.979164837438946),(1.,1.)))
REPRESENTATION_ITEM('')
SURFACE()
);
#207=(
BOUNDED_SURFACE()
B_SPLINE_SURFACE(3,1,((#33093,#33094),(#33095,#33096),(#33097,#33098),(#33099,
#33100)),.UNSPECIFIED.,.F.,.F.,.F.)
B_SPLINE_SURFACE_WITH_KNOTS((4,4),(2,2),(0.,1.),(0.,1.),.UNSPECIFIED.)
GEOMETRIC_REPRESENTATION_ITEM()
RATIONAL_B_SPLINE_SURFACE(((1.,1.),(0.97852393395982,0.98163056167315),
(0.97852393395982,0.98163056167315),(1.,1.)))
REPRESENTATION_ITEM('')
SURFACE()
);
#208=(
BOUNDED_SURFACE()
B_SPLINE_SURFACE(3,1,((#33115,#33116),(#33117,#33118),(#33119,#33120),(#33121,
#33122)),.UNSPECIFIED.,.F.,.F.,.F.)
B_SPLINE_SURFACE_WITH_KNOTS((4,4),(2,2),(0.,1.),(0.,0.960625757105633),
 .UNSPECIFIED.)
GEOMETRIC_REPRESENTATION_ITEM()
RATIONAL_B_SPLINE_SURFACE(((1.,1.),(0.969713710620478,0.979821031654969),
(0.969713710620478,0.979821031654969),(1.,1.)))
REPRESENTATION_ITEM('')
SURFACE()
);
#209=(
BOUNDED_SURFACE()
B_SPLINE_SURFACE(3,1,((#33145,#33146),(#33147,#33148),(#33149,#33150),(#33151,
#33152)),.UNSPECIFIED.,.F.,.F.,.F.)
B_SPLINE_SURFACE_WITH_KNOTS((4,4),(2,2),(0.,1.),(0.,1.),.UNSPECIFIED.)
GEOMETRIC_REPRESENTATION_ITEM()
RATIONAL_B_SPLINE_SURFACE(((1.,1.),(0.978523933959819,0.981630561673153),
(0.978523933959819,0.981630561673153),(1.,1.)))
REPRESENTATION_ITEM('')
SURFACE()
);
#210=(
BOUNDED_SURFACE()
B_SPLINE_SURFACE(3,1,((#33167,#33168),(#33169,#33170),(#33171,#33172),(#33173,
#33174)),.UNSPECIFIED.,.F.,.F.,.F.)
B_SPLINE_SURFACE_WITH_KNOTS((4,4),(2,2),(0.,1.),(0.,0.966511290545776),
 .UNSPECIFIED.)
GEOMETRIC_REPRESENTATION_ITEM()
RATIONAL_B_SPLINE_SURFACE(((1.,1.),(0.969175395688119,0.979164837438949),
(0.969175395688119,0.979164837438949),(1.,1.)))
REPRESENTATION_ITEM('')
SURFACE()
);
#211=(
BOUNDED_SURFACE()
B_SPLINE_SURFACE(3,1,((#33197,#33198),(#33199,#33200),(#33201,#33202),(#33203,
#33204)),.UNSPECIFIED.,.F.,.F.,.F.)
B_SPLINE_SURFACE_WITH_KNOTS((4,4),(2,2),(0.633798356768784,1.),(0.,1.),
 .UNSPECIFIED.)
GEOMETRIC_REPRESENTATION_ITEM()
RATIONAL_B_SPLINE_SURFACE(((0.791490742148516,0.816755884976974),(0.820835717853236,
0.842545119271855),(0.890338803803731,0.903626490946197),(1.,1.)))
REPRESENTATION_ITEM('')
SURFACE()
);
#212=(
BOUNDED_SURFACE()
B_SPLINE_SURFACE(3,1,((#33226,#33227,#33228,#33229),(#33230,#33231,#33232,
#33233),(#33234,#33235,#33236,#33237),(#33238,#33239,#33240,#33241)),
 .UNSPECIFIED.,.F.,.F.,.F.)
B_SPLINE_SURFACE_WITH_KNOTS((4,4),(2,1,1,2),(0.,0.152025639047805),(-0.000385633117440705,
0.,1.,1.001),.UNSPECIFIED.)
GEOMETRIC_REPRESENTATION_ITEM()
RATIONAL_B_SPLINE_SURFACE(((1.,1.,1.,1.),(0.999893343135597,0.999893343135597,
0.997697021403987,0.997697021403987),(0.999802900849163,0.999802900849163,
0.995744154600747,0.995744154600747),(0.9997286731407,0.9997286731407,0.994141399590279,
0.994141399590279)))
REPRESENTATION_ITEM('')
SURFACE()
);
#213=(
BOUNDED_SURFACE()
B_SPLINE_SURFACE(3,1,((#33248,#33249),(#33250,#33251),(#33252,#33253),(#33254,
#33255)),.UNSPECIFIED.,.F.,.F.,.F.)
B_SPLINE_SURFACE_WITH_KNOTS((4,4),(2,2),(0.,1.),(1.,1.00115361672614),
 .UNSPECIFIED.)
GEOMETRIC_REPRESENTATION_ITEM()
RATIONAL_B_SPLINE_SURFACE(((1.,1.),(0.975189339715083,0.975189339715083),
(0.975189339715083,0.975189339715083),(1.,1.)))
REPRESENTATION_ITEM('')
SURFACE()
);
#214=(
BOUNDED_SURFACE()
B_SPLINE_SURFACE(3,1,((#33256,#33257,#33258,#33259),(#33260,#33261,#33262,
#33263),(#33264,#33265,#33266,#33267),(#33268,#33269,#33270,#33271),(#33272,
#33273,#33274,#33275),(#33276,#33277,#33278,#33279),(#33280,#33281,#33282,
#33283),(#33284,#33285,#33286,#33287),(#33288,#33289,#33290,#33291),(#33292,
#33293,#33294,#33295)),.UNSPECIFIED.,.F.,.F.,.F.)
B_SPLINE_SURFACE_WITH_KNOTS((4,3,3,4),(2,1,1,2),(-0.000651766775030853,
0.,1.,1.00065175575688),(-0.000817120226221179,0.,0.676109671237986,0.676119671237986),
 .UNSPECIFIED.)
GEOMETRIC_REPRESENTATION_ITEM()
RATIONAL_B_SPLINE_SURFACE(((1.,1.,1.,1.),(1.,1.,1.,1.),(1.,1.,1.,1.),(1.,
1.,1.,1.),(0.998736553042339,0.998736553042339,0.999455940415833,0.999455940415833),
(0.998736553042339,0.998736553042339,0.999455940415833,0.999455940415833),
(1.,1.,1.,1.),(1.,1.,1.,1.),(1.,1.,1.,1.),(1.,1.,1.,1.)))
REPRESENTATION_ITEM('')
SURFACE()
);
#215=(
BOUNDED_SURFACE()
B_SPLINE_SURFACE(3,1,((#33318,#33319),(#33320,#33321),(#33322,#33323),(#33324,
#33325)),.UNSPECIFIED.,.F.,.F.,.F.)
B_SPLINE_SURFACE_WITH_KNOTS((4,4),(2,2),(0.,1.),(1.,1.00127139915746),
 .UNSPECIFIED.)
GEOMETRIC_REPRESENTATION_ITEM()
RATIONAL_B_SPLINE_SURFACE(((1.,1.),(0.975189339715083,0.975189339715083),
(0.975189339715083,0.975189339715083),(1.,1.)))
REPRESENTATION_ITEM('')
SURFACE()
);
#216=(
BOUNDED_SURFACE()
B_SPLINE_SURFACE(3,1,((#33333,#33334,#33335,#33336),(#33337,#33338,#33339,
#33340),(#33341,#33342,#33343,#33344),(#33345,#33346,#33347,#33348),(#33349,
#33350,#33351,#33352),(#33353,#33354,#33355,#33356),(#33357,#33358,#33359,
#33360)),.UNSPECIFIED.,.F.,.F.,.F.)
B_SPLINE_SURFACE_WITH_KNOTS((4,3,4),(2,1,1,2),(0.,0.15224442477612,0.152293862972879),
(-0.000531337228447352,0.,1.,1.001),.UNSPECIFIED.)
GEOMETRIC_REPRESENTATION_ITEM()
RATIONAL_B_SPLINE_SURFACE(((1.,1.,1.,1.),(0.999893154836255,0.999893154836255,
0.997693707102185,0.997693707102186),(0.999802576253004,0.999802576253004,
0.995738534439964,0.995738534439964),(0.999728264250248,0.999728264250248,
0.994134482013335,0.994134482013335),(0.999728264250248,0.999728264250248,
0.994134482013335,0.994134482013335),(0.999728264250248,0.999728264250248,
0.994134482013335,0.994134482013335),(0.999728264250248,0.999728264250248,
0.994134482013335,0.994134482013335)))
REPRESENTATION_ITEM('')
SURFACE()
);
#217=(
BOUNDED_SURFACE()
B_SPLINE_SURFACE(3,1,((#33373,#33374,#33375,#33376),(#33377,#33378,#33379,
#33380),(#33381,#33382,#33383,#33384),(#33385,#33386,#33387,#33388)),
 .UNSPECIFIED.,.F.,.F.,.F.)
B_SPLINE_SURFACE_WITH_KNOTS((4,4),(2,1,1,2),(0.847755575223898,1.),(-0.000531332476382396,
0.,1.,1.001),.UNSPECIFIED.)
GEOMETRIC_REPRESENTATION_ITEM()
RATIONAL_B_SPLINE_SURFACE(((0.999728264250248,0.999728264250248,0.994134482013336,
0.994134482013336),(0.999802576253004,0.999802576253004,0.995738534439964,
0.995738534439964),(0.999893154836255,0.999893154836255,0.997693707102186,
0.997693707102186),(1.,1.,1.,1.)))
REPRESENTATION_ITEM('')
SURFACE()
);
#218=(
BOUNDED_SURFACE()
B_SPLINE_SURFACE(3,1,((#33391,#33392,#33393,#33394),(#33395,#33396,#33397,
#33398),(#33399,#33400,#33401,#33402),(#33403,#33404,#33405,#33406)),
 .UNSPECIFIED.,.F.,.F.,.F.)
B_SPLINE_SURFACE_WITH_KNOTS((4,4),(2,1,1,2),(0.365923647633872,0.36753176510902),
(-0.000355481502485282,0.,1.,1.0002958898079),.UNSPECIFIED.)
GEOMETRIC_REPRESENTATION_ITEM()
RATIONAL_B_SPLINE_SURFACE(((0.791557641756873,0.791557641756873,0.816814678335385,
0.816814678335385),(0.791557641756873,0.791557641756873,0.816814678335385,
0.816814678335385),(0.791557641756873,0.791557641756873,0.816814678335385,
0.816814678335385),(0.791557641756873,0.791557641756873,0.816814678335385,
0.816814678335385)))
REPRESENTATION_ITEM('')
SURFACE()
);
#219=(
BOUNDED_SURFACE()
B_SPLINE_SURFACE(3,1,((#33407,#33408),(#33409,#33410),(#33411,#33412),(#33413,
#33414)),.UNSPECIFIED.,.F.,.F.,.F.)
B_SPLINE_SURFACE_WITH_KNOTS((4,4),(2,2),(0.,1.),(0.,0.966044174191949),
 .UNSPECIFIED.)
GEOMETRIC_REPRESENTATION_ITEM()
RATIONAL_B_SPLINE_SURFACE(((1.,1.),(0.969175395688119,0.979160009526791),
(0.969175395688119,0.979160009526791),(1.,1.)))
REPRESENTATION_ITEM('')
SURFACE()
);
#220=(
BOUNDED_SURFACE()
B_SPLINE_SURFACE(3,1,((#33423,#33424),(#33425,#33426),(#33427,#33428),(#33429,
#33430)),.UNSPECIFIED.,.F.,.F.,.F.)
B_SPLINE_SURFACE_WITH_KNOTS((4,4),(2,2),(0.,1.),(0.,1.),.UNSPECIFIED.)
GEOMETRIC_REPRESENTATION_ITEM()
RATIONAL_B_SPLINE_SURFACE(((1.,1.),(0.97852393395982,0.98163056167315),
(0.97852393395982,0.98163056167315),(1.,1.)))
REPRESENTATION_ITEM('')
SURFACE()
);
#221=(
BOUNDED_SURFACE()
B_SPLINE_SURFACE(3,1,((#33432,#33433),(#33434,#33435),(#33436,#33437),(#33438,
#33439)),.UNSPECIFIED.,.F.,.F.,.F.)
B_SPLINE_SURFACE_WITH_KNOTS((4,4),(2,2),(0.,1.),(0.,0.960122375136112),
 .UNSPECIFIED.)
GEOMETRIC_REPRESENTATION_ITEM()
RATIONAL_B_SPLINE_SURFACE(((1.,1.),(0.969713710620478,0.979815735270679),
(0.969713710620478,0.979815735270679),(1.,1.)))
REPRESENTATION_ITEM('')
SURFACE()
);
#222=(
BOUNDED_SURFACE()
B_SPLINE_SURFACE(3,1,((#33448,#33449),(#33450,#33451),(#33452,#33453),(#33454,
#33455)),.UNSPECIFIED.,.F.,.F.,.F.)
B_SPLINE_SURFACE_WITH_KNOTS((4,4),(2,2),(0.,1.),(0.,1.),.UNSPECIFIED.)
GEOMETRIC_REPRESENTATION_ITEM()
RATIONAL_B_SPLINE_SURFACE(((1.,1.),(0.978523933959819,0.981630561673153),
(0.978523933959819,0.981630561673153),(1.,1.)))
REPRESENTATION_ITEM('')
SURFACE()
);
#223=(
BOUNDED_SURFACE()
B_SPLINE_SURFACE(3,1,((#33457,#33458),(#33459,#33460),(#33461,#33462),(#33463,
#33464)),.UNSPECIFIED.,.F.,.F.,.F.)
B_SPLINE_SURFACE_WITH_KNOTS((4,4),(2,2),(0.,1.),(0.,0.966044174191933),
 .UNSPECIFIED.)
GEOMETRIC_REPRESENTATION_ITEM()
RATIONAL_B_SPLINE_SURFACE(((1.,1.),(0.969175395688119,0.979160009526794),
(0.969175395688119,0.979160009526794),(1.,1.)))
REPRESENTATION_ITEM('')
SURFACE()
);
#224=(
BOUNDED_SURFACE()
B_SPLINE_SURFACE(3,1,((#33466,#33467),(#33468,#33469),(#33470,#33471),(#33472,
#33473)),.UNSPECIFIED.,.F.,.F.,.F.)
B_SPLINE_SURFACE_WITH_KNOTS((4,4),(2,2),(0.634076354292062,1.),(0.,1.),
 .UNSPECIFIED.)
GEOMETRIC_REPRESENTATION_ITEM()
RATIONAL_B_SPLINE_SURFACE(((0.791557642220831,0.816814678743125),(0.820941265840603,
0.842637877971094),(0.890422051766993,0.903699651723386),(1.,1.)))
REPRESENTATION_ITEM('')
SURFACE()
);
#225=(
BOUNDED_SURFACE()
B_SPLINE_SURFACE(3,1,((#33474,#33475),(#33476,#33477),(#33478,#33479),(#33480,
#33481)),.UNSPECIFIED.,.F.,.F.,.F.)
B_SPLINE_SURFACE_WITH_KNOTS((4,4),(2,2),(0.,1.),(1.,1.00115971095081),
 .UNSPECIFIED.)
GEOMETRIC_REPRESENTATION_ITEM()
RATIONAL_B_SPLINE_SURFACE(((1.,1.),(0.975189339715083,0.975189339715083),
(0.975189339715083,0.975189339715083),(1.,1.)))
REPRESENTATION_ITEM('')
SURFACE()
);
#226=(
BOUNDED_SURFACE()
B_SPLINE_SURFACE(3,1,((#33482,#33483),(#33484,#33485),(#33486,#33487),(#33488,
#33489),(#33490,#33491),(#33492,#33493),(#33494,#33495),(#33496,#33497),
(#33498,#33499),(#33500,#33501)),.UNSPECIFIED.,.F.,.F.,.F.)
B_SPLINE_SURFACE_WITH_KNOTS((4,3,3,4),(2,2),(-0.000658266375657395,0.,1.,
1.00065830337858),(-0.000823662838273568,0.),.UNSPECIFIED.)
GEOMETRIC_REPRESENTATION_ITEM()
RATIONAL_B_SPLINE_SURFACE(((1.,1.),(1.,1.),(1.,1.),(1.,1.),(0.998672257010864,
0.998672257010864),(0.998672257010864,0.998672257010864),(1.,1.),(1.,1.),
(1.,1.),(1.,1.)))
REPRESENTATION_ITEM('')
SURFACE()
);
#227=(
BOUNDED_SURFACE()
B_SPLINE_SURFACE(3,1,((#33526,#33527),(#33528,#33529),(#33530,#33531),(#33532,
#33533)),.UNSPECIFIED.,.F.,.F.,.F.)
B_SPLINE_SURFACE_WITH_KNOTS((4,4),(2,2),(0.,1.),(-0.000998381213712629,
0.),.UNSPECIFIED.)
GEOMETRIC_REPRESENTATION_ITEM()
RATIONAL_B_SPLINE_SURFACE(((1.,1.),(0.978516115582536,0.978516115582536),
(0.978516115582536,0.978516115582536),(1.,1.)))
REPRESENTATION_ITEM('')
SURFACE()
);
#228=(
BOUNDED_SURFACE()
B_SPLINE_SURFACE(3,1,((#34127,#34128,#34129,#34130),(#34131,#34132,#34133,
#34134),(#34135,#34136,#34137,#34138),(#34139,#34140,#34141,#34142),(#34143,
#34144,#34145,#34146),(#34147,#34148,#34149,#34150),(#34151,#34152,#34153,
#34154),(#34155,#34156,#34157,#34158),(#34159,#34160,#34161,#34162),(#34163,
#34164,#34165,#34166)),.UNSPECIFIED.,.F.,.F.,.F.)
B_SPLINE_SURFACE_WITH_KNOTS((4,3,3,4),(2,1,1,2),(-0.001,0.,0.205321724422313,
0.206321724412313),(-0.000396813100233054,0.,1.,1.001),.UNSPECIFIED.)
GEOMETRIC_REPRESENTATION_ITEM()
RATIONAL_B_SPLINE_SURFACE(((1.,1.,1.,1.),(1.,1.,1.,1.),(1.,1.,1.,1.),(1.,
1.,1.,1.),(0.996948890458759,0.996948890458759,0.996889659273247,0.996889659273247),
(0.994524239989928,0.994524239989928,0.994417939068052,0.994417939068052),
(0.992726048593505,0.992726048593505,0.992584839384415,0.992584839384415),
(0.992726048593505,0.992726048593505,0.992584839384415,0.992584839384415),
(0.992726048593505,0.992726048593505,0.992584839384415,0.992584839384415),
(0.992726048593505,0.992726048593505,0.992584839384415,0.992584839384415)))
REPRESENTATION_ITEM('')
SURFACE()
);
#229=(
BOUNDED_SURFACE()
B_SPLINE_SURFACE(3,1,((#35952,#35953),(#35954,#35955),(#35956,#35957),(#35958,
#35959),(#35960,#35961),(#35962,#35963),(#35964,#35965)),.UNSPECIFIED.,
 .F.,.F.,.F.)
B_SPLINE_SURFACE_WITH_KNOTS((4,3,4),(2,2),(0.,1.,1.00008671004856),(0.,
0.740226077012249),.UNSPECIFIED.)
GEOMETRIC_REPRESENTATION_ITEM()
RATIONAL_B_SPLINE_SURFACE(((1.,1.),(0.998672257010864,0.999507458473034),
(0.998672257010864,0.999507458473034),(1.,1.),(1.,1.),(1.,1.),(1.,1.)))
REPRESENTATION_ITEM('')
SURFACE()
);
#230=(
BOUNDED_SURFACE()
B_SPLINE_SURFACE(3,1,((#35978,#35979),(#35980,#35981),(#35982,#35983),(#35984,
#35985)),.UNSPECIFIED.,.F.,.F.,.F.)
B_SPLINE_SURFACE_WITH_KNOTS((4,4),(2,2),(0.,1.),(0.,1.),.UNSPECIFIED.)
GEOMETRIC_REPRESENTATION_ITEM()
RATIONAL_B_SPLINE_SURFACE(((1.,1.),(0.962057791684876,0.975189339715083),
(0.962057791684876,0.975189339715083),(1.,1.)))
REPRESENTATION_ITEM('')
SURFACE()
);
#231=(
BOUNDED_SURFACE()
B_SPLINE_SURFACE(3,1,((#35998,#35999,#36000,#36001),(#36002,#36003,#36004,
#36005),(#36006,#36007,#36008,#36009),(#36010,#36011,#36012,#36013)),
 .UNSPECIFIED.,.F.,.F.,.F.)
B_SPLINE_SURFACE_WITH_KNOTS((4,4),(2,1,1,2),(0.,0.152244424776119),(-0.000281365801619608,
0.,1.,1.001),.UNSPECIFIED.)
GEOMETRIC_REPRESENTATION_ITEM()
RATIONAL_B_SPLINE_SURFACE(((1.,1.,1.,1.),(0.999893154836255,0.999893154836255,
0.997693707102186,0.997693707102186),(0.999802576253004,0.999802576253004,
0.995738534439964,0.995738534439964),(0.999728264250248,0.999728264250248,
0.994134482013336,0.994134482013336)))
REPRESENTATION_ITEM('')
SURFACE()
);
#232=(
BOUNDED_SURFACE()
B_SPLINE_SURFACE(3,1,((#36027,#36028,#36029,#36030),(#36031,#36032,#36033,
#36034),(#36035,#36036,#36037,#36038),(#36039,#36040,#36041,#36042)),
 .UNSPECIFIED.,.F.,.F.,.F.)
B_SPLINE_SURFACE_WITH_KNOTS((4,4),(2,1,1,2),(0.847755575223896,1.),(-0.000269810410367957,
0.,1.,1.001),.UNSPECIFIED.)
GEOMETRIC_REPRESENTATION_ITEM()
RATIONAL_B_SPLINE_SURFACE(((0.999728264250248,0.999728264250248,0.994134482013336,
0.994134482013336),(0.999802576253004,0.999802576253004,0.995738534439964,
0.995738534439964),(0.999893154836255,0.999893154836255,0.997693707102186,
0.997693707102186),(1.,1.,1.,1.)))
REPRESENTATION_ITEM('')
SURFACE()
);
#233=(
BOUNDED_SURFACE()
B_SPLINE_SURFACE(3,1,((#36063,#36064),(#36065,#36066),(#36067,#36068),(#36069,
#36070)),.UNSPECIFIED.,.F.,.F.,.F.)
B_SPLINE_SURFACE_WITH_KNOTS((4,4),(2,2),(0.,0.365923648059291),(0.,1.),
 .UNSPECIFIED.)
GEOMETRIC_REPRESENTATION_ITEM()
RATIONAL_B_SPLINE_SURFACE(((1.,1.),(0.890422051062866,0.903699651104578),
(0.820941264947662,0.842637877186351),(0.79155764165439,0.816814678245319)))
REPRESENTATION_ITEM('')
SURFACE()
);
#234=(
BOUNDED_SURFACE()
B_SPLINE_SURFACE(3,1,((#36085,#36086),(#36087,#36088),(#36089,#36090),(#36091,
#36092)),.UNSPECIFIED.,.F.,.F.,.F.)
B_SPLINE_SURFACE_WITH_KNOTS((4,4),(2,2),(0.,1.),(0.,0.966044174191948),
 .UNSPECIFIED.)
GEOMETRIC_REPRESENTATION_ITEM()
RATIONAL_B_SPLINE_SURFACE(((1.,1.),(0.969175395688119,0.979160009526791),
(0.969175395688119,0.979160009526791),(1.,1.)))
REPRESENTATION_ITEM('')
SURFACE()
);
#235=(
BOUNDED_SURFACE()
B_SPLINE_SURFACE(3,1,((#36115,#36116),(#36117,#36118),(#36119,#36120),(#36121,
#36122)),.UNSPECIFIED.,.F.,.F.,.F.)
B_SPLINE_SURFACE_WITH_KNOTS((4,4),(2,2),(0.,1.),(0.,1.),.UNSPECIFIED.)
GEOMETRIC_REPRESENTATION_ITEM()
RATIONAL_B_SPLINE_SURFACE(((1.,1.),(0.97852393395982,0.98163056167315),
(0.97852393395982,0.98163056167315),(1.,1.)))
REPRESENTATION_ITEM('')
SURFACE()
);
#236=(
BOUNDED_SURFACE()
B_SPLINE_SURFACE(3,1,((#36137,#36138),(#36139,#36140),(#36141,#36142),(#36143,
#36144)),.UNSPECIFIED.,.F.,.F.,.F.)
B_SPLINE_SURFACE_WITH_KNOTS((4,4),(2,2),(0.,1.),(0.,0.960122375136112),
 .UNSPECIFIED.)
GEOMETRIC_REPRESENTATION_ITEM()
RATIONAL_B_SPLINE_SURFACE(((1.,1.),(0.969713710620478,0.979815735270679),
(0.969713710620478,0.979815735270679),(1.,1.)))
REPRESENTATION_ITEM('')
SURFACE()
);
#237=(
BOUNDED_SURFACE()
B_SPLINE_SURFACE(3,1,((#36167,#36168),(#36169,#36170),(#36171,#36172),(#36173,
#36174)),.UNSPECIFIED.,.F.,.F.,.F.)
B_SPLINE_SURFACE_WITH_KNOTS((4,4),(2,2),(0.,1.),(0.,1.),.UNSPECIFIED.)
GEOMETRIC_REPRESENTATION_ITEM()
RATIONAL_B_SPLINE_SURFACE(((1.,1.),(0.978523933959819,0.981630561673153),
(0.978523933959819,0.981630561673153),(1.,1.)))
REPRESENTATION_ITEM('')
SURFACE()
);
#238=(
BOUNDED_SURFACE()
B_SPLINE_SURFACE(3,1,((#36189,#36190),(#36191,#36192),(#36193,#36194),(#36195,
#36196)),.UNSPECIFIED.,.F.,.F.,.F.)
B_SPLINE_SURFACE_WITH_KNOTS((4,4),(2,2),(0.,1.),(0.,0.966044174191938),
 .UNSPECIFIED.)
GEOMETRIC_REPRESENTATION_ITEM()
RATIONAL_B_SPLINE_SURFACE(((1.,1.),(0.969175395688119,0.979160009526794),
(0.969175395688119,0.979160009526794),(1.,1.)))
REPRESENTATION_ITEM('')
SURFACE()
);
#239=(
BOUNDED_SURFACE()
B_SPLINE_SURFACE(3,1,((#36209,#36210),(#36211,#36212),(#36213,#36214),(#36215,
#36216)),.UNSPECIFIED.,.F.,.F.,.F.)
B_SPLINE_SURFACE_WITH_KNOTS((4,4),(2,2),(0.634076354292045,1.),(0.,1.),
 .UNSPECIFIED.)
GEOMETRIC_REPRESENTATION_ITEM()
RATIONAL_B_SPLINE_SURFACE(((0.791557642220827,0.816814678743122),(0.820941265840597,
0.842637877971089),(0.890422051766988,0.903699651723381),(1.,1.)))
REPRESENTATION_ITEM('')
SURFACE()
);
#240=(
BOUNDED_SURFACE()
B_SPLINE_SURFACE(3,2,((#38724,#38725,#38726),(#38727,#38728,#38729),(#38730,
#38731,#38732),(#38733,#38734,#38735),(#38736,#38737,#38738),(#38739,#38740,
#38741)),.UNSPECIFIED.,.F.,.F.,.F.)
B_SPLINE_SURFACE_WITH_KNOTS((4,2,4),(3,3),(7.24208658159082,7.54803410778265,
7.85398163397448),(0.,1.),.UNSPECIFIED.)
GEOMETRIC_REPRESENTATION_ITEM()
RATIONAL_B_SPLINE_SURFACE(((1.,0.913794834970588,1.),(1.,0.940095751976153,
1.),(1.,0.962067838102692,1.),(1.,0.992046010392396,1.),(1.,1.00005792034581,
1.),(1.,1.,1.)))
REPRESENTATION_ITEM('')
SURFACE()
);
#241=(
BOUNDED_SURFACE()
B_SPLINE_SURFACE(3,2,((#38904,#38905,#38906),(#38907,#38908,#38909),(#38910,
#38911,#38912),(#38913,#38914,#38915),(#38916,#38917,#38918),(#38919,#38920,
#38921)),.UNSPECIFIED.,.F.,.F.,.F.)
B_SPLINE_SURFACE_WITH_KNOTS((4,2,4),(3,3),(7.2420865815908,7.54803410778264,
7.85398163397448),(0.,1.),.UNSPECIFIED.)
GEOMETRIC_REPRESENTATION_ITEM()
RATIONAL_B_SPLINE_SURFACE(((1.,0.913794834970583,1.),(1.,0.94009575197619,
1.),(1.,0.962067838102636,1.),(1.,0.99204601039245,1.),(1.,1.00005792034577,
1.),(1.,1.,1.)))
REPRESENTATION_ITEM('')
SURFACE()
);
#242=(
BOUNDED_SURFACE()
B_SPLINE_SURFACE(3,2,((#39155,#39156,#39157),(#39158,#39159,#39160),(#39161,
#39162,#39163),(#39164,#39165,#39166),(#39167,#39168,#39169),(#39170,#39171,
#39172)),.UNSPECIFIED.,.F.,.F.,.F.)
B_SPLINE_SURFACE_WITH_KNOTS((4,2,4),(3,3),(7.24208658159082,7.54803410778265,
7.85398163397448),(0.,1.),.UNSPECIFIED.)
GEOMETRIC_REPRESENTATION_ITEM()
RATIONAL_B_SPLINE_SURFACE(((1.,0.913794834970588,1.),(1.,0.940095751976173,
1.),(1.,0.962067838102665,1.),(1.,0.992046010392423,1.),(1.,1.00005792034579,
1.),(1.,1.,1.)))
REPRESENTATION_ITEM('')
SURFACE()
);
#243=(
BOUNDED_SURFACE()
B_SPLINE_SURFACE(3,2,((#39243,#39244,#39245),(#39246,#39247,#39248),(#39249,
#39250,#39251),(#39252,#39253,#39254),(#39255,#39256,#39257),(#39258,#39259,
#39260)),.UNSPECIFIED.,.F.,.F.,.F.)
B_SPLINE_SURFACE_WITH_KNOTS((4,2,4),(3,3),(7.2420865815908,7.54803410778264,
7.85398163397448),(0.,1.),.UNSPECIFIED.)
GEOMETRIC_REPRESENTATION_ITEM()
RATIONAL_B_SPLINE_SURFACE(((1.,0.913794834970582,1.),(1.,0.94009575197617,
1.),(1.,0.962067838102664,1.),(1.,0.992046010392423,1.),(1.,1.00005792034579,
1.),(1.,1.,1.)))
REPRESENTATION_ITEM('')
SURFACE()
);
#244=B_SPLINE_SURFACE_WITH_KNOTS('',3,1,((#26297,#26298),(#26299,#26300),
(#26301,#26302),(#26303,#26304),(#26305,#26306),(#26307,#26308),(#26309,
#26310),(#26311,#26312),(#26313,#26314),(#26315,#26316)),.UNSPECIFIED.,
 .F.,.F.,.F.,(4,2,2,2,4),(2,2),(0.5,0.625,0.75,0.875,1.),(0.,1.),
 .UNSPECIFIED.);
#245=B_SPLINE_SURFACE_WITH_KNOTS('',3,1,((#26363,#26364),(#26365,#26366),
(#26367,#26368),(#26369,#26370),(#26371,#26372),(#26373,#26374),(#26375,
#26376),(#26377,#26378),(#26379,#26380),(#26381,#26382),(#26383,#26384),
(#26385,#26386)),.UNSPECIFIED.,.F.,.F.,.F.,(4,2,2,2,2,4),(2,2),(0.,0.125,
0.25,0.375,0.5,0.503056895069501),(0.,1.),.UNSPECIFIED.);
#246=B_SPLINE_SURFACE_WITH_KNOTS('',3,1,((#27108,#27109),(#27110,#27111),
(#27112,#27113),(#27114,#27115),(#27116,#27117),(#27118,#27119),(#27120,
#27121),(#27122,#27123),(#27124,#27125),(#27126,#27127)),.UNSPECIFIED.,
 .F.,.F.,.F.,(4,2,2,2,4),(2,2),(0.5,0.625,0.75,0.875,1.00000000012908),
(0.,1.),.UNSPECIFIED.);
#247=B_SPLINE_SURFACE_WITH_KNOTS('',3,1,((#27130,#27131),(#27132,#27133),
(#27134,#27135),(#27136,#27137),(#27138,#27139),(#27140,#27141),(#27142,
#27143),(#27144,#27145),(#27146,#27147),(#27148,#27149),(#27150,#27151),
(#27152,#27153)),.UNSPECIFIED.,.F.,.F.,.F.,(4,2,2,2,2,4),(2,2),(0.,0.125,
0.25,0.375,0.5,0.50305689506972),(0.,1.),.UNSPECIFIED.);
#248=B_SPLINE_SURFACE_WITH_KNOTS('',3,1,((#33564,#33565,#33566,#33567),
(#33568,#33569,#33570,#33571),(#33572,#33573,#33574,#33575),(#33576,#33577,
#33578,#33579),(#33580,#33581,#33582,#33583),(#33584,#33585,#33586,#33587),
(#33588,#33589,#33590,#33591),(#33592,#33593,#33594,#33595),(#33596,#33597,
#33598,#33599),(#33600,#33601,#33602,#33603),(#33604,#33605,#33606,#33607),
(#33608,#33609,#33610,#33611),(#33612,#33613,#33614,#33615),(#33616,#33617,
#33618,#33619),(#33620,#33621,#33622,#33623),(#33624,#33625,#33626,#33627)),
 .UNSPECIFIED.,.F.,.F.,.F.,(4,3,2,2,2,3,4),(2,1,1,2),(-0.00031432553449176,
0.,0.125,0.25,0.375,0.418191871014293,0.418392704999572),(-0.000189913748737528,
0.,1.,1.00033781779361),.UNSPECIFIED.);
#249=B_SPLINE_SURFACE_WITH_KNOTS('',3,1,((#33642,#33643,#33644,#33645),
(#33646,#33647,#33648,#33649),(#33650,#33651,#33652,#33653),(#33654,#33655,
#33656,#33657),(#33658,#33659,#33660,#33661),(#33662,#33663,#33664,#33665),
(#33666,#33667,#33668,#33669),(#33670,#33671,#33672,#33673),(#33674,#33675,
#33676,#33677),(#33678,#33679,#33680,#33681),(#33682,#33683,#33684,#33685),
(#33686,#33687,#33688,#33689),(#33690,#33691,#33692,#33693),(#33694,#33695,
#33696,#33697),(#33698,#33699,#33700,#33701),(#33702,#33703,#33704,#33705)),
 .UNSPECIFIED.,.F.,.F.,.F.,(4,3,2,2,2,3,4),(2,1,1,2),(-0.00221274313418469,
0.,0.25,0.5,0.75,1.,1.00210632487476),(-0.00205770015535969,0.,0.975652891172124,
0.976690614800578),.UNSPECIFIED.);
#250=B_SPLINE_SURFACE_WITH_KNOTS('',3,1,((#33724,#33725,#33726,#33727),
(#33728,#33729,#33730,#33731),(#33732,#33733,#33734,#33735),(#33736,#33737,
#33738,#33739),(#33740,#33741,#33742,#33743),(#33744,#33745,#33746,#33747),
(#33748,#33749,#33750,#33751),(#33752,#33753,#33754,#33755),(#33756,#33757,
#33758,#33759),(#33760,#33761,#33762,#33763),(#33764,#33765,#33766,#33767),
(#33768,#33769,#33770,#33771),(#33772,#33773,#33774,#33775),(#33776,#33777,
#33778,#33779),(#33780,#33781,#33782,#33783),(#33784,#33785,#33786,#33787)),
 .UNSPECIFIED.,.F.,.F.,.F.,(4,3,2,2,2,3,4),(2,1,1,2),(-0.00236149222569652,
0.,0.25,0.5,0.75,1.,1.00236149222657),(-0.00220329632355928,0.,1.,1.00136244470998),
 .UNSPECIFIED.);
#251=B_SPLINE_SURFACE_WITH_KNOTS('',3,1,((#33802,#33803,#33804,#33805),
(#33806,#33807,#33808,#33809),(#33810,#33811,#33812,#33813),(#33814,#33815,
#33816,#33817),(#33818,#33819,#33820,#33821),(#33822,#33823,#33824,#33825),
(#33826,#33827,#33828,#33829),(#33830,#33831,#33832,#33833),(#33834,#33835,
#33836,#33837),(#33838,#33839,#33840,#33841),(#33842,#33843,#33844,#33845),
(#33846,#33847,#33848,#33849),(#33850,#33851,#33852,#33853),(#33854,#33855,
#33856,#33857),(#33858,#33859,#33860,#33861),(#33862,#33863,#33864,#33865)),
 .UNSPECIFIED.,.F.,.F.,.F.,(4,3,2,2,2,3,4),(2,1,1,2),(-0.00193140008151945,
0.,0.25,0.5,0.75,1.,1.00183441898671),(-0.00178369340673476,0.,0.978636855822753,
0.979556967191144),.UNSPECIFIED.);
#252=B_SPLINE_SURFACE_WITH_KNOTS('',3,1,((#33884,#33885,#33886,#33887),
(#33888,#33889,#33890,#33891),(#33892,#33893,#33894,#33895),(#33896,#33897,
#33898,#33899),(#33900,#33901,#33902,#33903),(#33904,#33905,#33906,#33907),
(#33908,#33909,#33910,#33911),(#33912,#33913,#33914,#33915),(#33916,#33917,
#33918,#33919),(#33920,#33921,#33922,#33923),(#33924,#33925,#33926,#33927),
(#33928,#33929,#33930,#33931),(#33932,#33933,#33934,#33935),(#33936,#33937,
#33938,#33939),(#33940,#33941,#33942,#33943),(#33944,#33945,#33946,#33947)),
 .UNSPECIFIED.,.F.,.F.,.F.,(4,3,2,2,2,3,4),(2,1,1,2),(-0.00236149222579484,
0.,0.25,0.5,0.75,1.,1.00236149222666),(-0.00220329632365572,0.,1.,1.00131125111415),
 .UNSPECIFIED.);
#253=B_SPLINE_SURFACE_WITH_KNOTS('',3,1,((#33962,#33963,#33964,#33965),
(#33966,#33967,#33968,#33969),(#33970,#33971,#33972,#33973),(#33974,#33975,
#33976,#33977),(#33978,#33979,#33980,#33981),(#33982,#33983,#33984,#33985),
(#33986,#33987,#33988,#33989),(#33990,#33991,#33992,#33993),(#33994,#33995,
#33996,#33997),(#33998,#33999,#34000,#34001),(#34002,#34003,#34004,#34005),
(#34006,#34007,#34008,#34009),(#34010,#34011,#34012,#34013),(#34014,#34015,
#34016,#34017),(#34018,#34019,#34020,#34021),(#34022,#34023,#34024,#34025)),
 .UNSPECIFIED.,.F.,.F.,.F.,(4,3,2,2,2,3,4),(2,1,1,2),(-0.00224555441012961,
0.,0.25,0.5,0.75,1.,1.00213171827197),(-0.00209030173265073,0.,0.975652891172124,
0.97673425926222),.UNSPECIFIED.);
#254=B_SPLINE_SURFACE_WITH_KNOTS('',3,1,((#34044,#34045,#34046,#34047),
(#34048,#34049,#34050,#34051),(#34052,#34053,#34054,#34055),(#34056,#34057,
#34058,#34059),(#34060,#34061,#34062,#34063),(#34064,#34065,#34066,#34067),
(#34068,#34069,#34070,#34071),(#34072,#34073,#34074,#34075),(#34076,#34077,
#34078,#34079),(#34080,#34081,#34082,#34083),(#34084,#34085,#34086,#34087),
(#34088,#34089,#34090,#34091),(#34092,#34093,#34094,#34095),(#34096,#34097,
#34098,#34099),(#34100,#34101,#34102,#34103),(#34104,#34105,#34106,#34107)),
 .UNSPECIFIED.,.F.,.F.,.F.,(4,3,2,2,2,3,4),(2,1,1,2),(0.581437458849578,
0.581806922548263,0.625,0.75,0.875,1.,1.00037830613069),(-0.000375883807932015,
0.,1.,1.00034850475001),.UNSPECIFIED.);
#255=B_SPLINE_SURFACE_WITH_KNOTS('',3,3,((#34263,#34264,#34265,#34266,#34267,
#34268,#34269,#34270,#34271,#34272,#34273,#34274,#34275,#34276,#34277,#34278,
#34279,#34280,#34281,#34282,#34283,#34284,#34285,#34286,#34287,#34288,#34289,
#34290,#34291,#34292,#34293,#34294,#34295,#34296,#34297,#34298,#34299,#34300,
#34301,#34302,#34303,#34304,#34305,#34306,#34307,#34308,#34309,#34310,#34311,
#34312,#34313,#34314,#34315,#34316),(#34317,#34318,#34319,#34320,#34321,
#34322,#34323,#34324,#34325,#34326,#34327,#34328,#34329,#34330,#34331,#34332,
#34333,#34334,#34335,#34336,#34337,#34338,#34339,#34340,#34341,#34342,#34343,
#34344,#34345,#34346,#34347,#34348,#34349,#34350,#34351,#34352,#34353,#34354,
#34355,#34356,#34357,#34358,#34359,#34360,#34361,#34362,#34363,#34364,#34365,
#34366,#34367,#34368,#34369,#34370),(#34371,#34372,#34373,#34374,#34375,
#34376,#34377,#34378,#34379,#34380,#34381,#34382,#34383,#34384,#34385,#34386,
#34387,#34388,#34389,#34390,#34391,#34392,#34393,#34394,#34395,#34396,#34397,
#34398,#34399,#34400,#34401,#34402,#34403,#34404,#34405,#34406,#34407,#34408,
#34409,#34410,#34411,#34412,#34413,#34414,#34415,#34416,#34417,#34418,#34419,
#34420,#34421,#34422,#34423,#34424),(#34425,#34426,#34427,#34428,#34429,
#34430,#34431,#34432,#34433,#34434,#34435,#34436,#34437,#34438,#34439,#34440,
#34441,#34442,#34443,#34444,#34445,#34446,#34447,#34448,#34449,#34450,#34451,
#34452,#34453,#34454,#34455,#34456,#34457,#34458,#34459,#34460,#34461,#34462,
#34463,#34464,#34465,#34466,#34467,#34468,#34469,#34470,#34471,#34472,#34473,
#34474,#34475,#34476,#34477,#34478),(#34479,#34480,#34481,#34482,#34483,
#34484,#34485,#34486,#34487,#34488,#34489,#34490,#34491,#34492,#34493,#34494,
#34495,#34496,#34497,#34498,#34499,#34500,#34501,#34502,#34503,#34504,#34505,
#34506,#34507,#34508,#34509,#34510,#34511,#34512,#34513,#34514,#34515,#34516,
#34517,#34518,#34519,#34520,#34521,#34522,#34523,#34524,#34525,#34526,#34527,
#34528,#34529,#34530,#34531,#34532),(#34533,#34534,#34535,#34536,#34537,
#34538,#34539,#34540,#34541,#34542,#34543,#34544,#34545,#34546,#34547,#34548,
#34549,#34550,#34551,#34552,#34553,#34554,#34555,#34556,#34557,#34558,#34559,
#34560,#34561,#34562,#34563,#34564,#34565,#34566,#34567,#34568,#34569,#34570,
#34571,#34572,#34573,#34574,#34575,#34576,#34577,#34578,#34579,#34580,#34581,
#34582,#34583,#34584,#34585,#34586),(#34587,#34588,#34589,#34590,#34591,
#34592,#34593,#34594,#34595,#34596,#34597,#34598,#34599,#34600,#34601,#34602,
#34603,#34604,#34605,#34606,#34607,#34608,#34609,#34610,#34611,#34612,#34613,
#34614,#34615,#34616,#34617,#34618,#34619,#34620,#34621,#34622,#34623,#34624,
#34625,#34626,#34627,#34628,#34629,#34630,#34631,#34632,#34633,#34634,#34635,
#34636,#34637,#34638,#34639,#34640),(#34641,#34642,#34643,#34644,#34645,
#34646,#34647,#34648,#34649,#34650,#34651,#34652,#34653,#34654,#34655,#34656,
#34657,#34658,#34659,#34660,#34661,#34662,#34663,#34664,#34665,#34666,#34667,
#34668,#34669,#34670,#34671,#34672,#34673,#34674,#34675,#34676,#34677,#34678,
#34679,#34680,#34681,#34682,#34683,#34684,#34685,#34686,#34687,#34688,#34689,
#34690,#34691,#34692,#34693,#34694),(#34695,#34696,#34697,#34698,#34699,
#34700,#34701,#34702,#34703,#34704,#34705,#34706,#34707,#34708,#34709,#34710,
#34711,#34712,#34713,#34714,#34715,#34716,#34717,#34718,#34719,#34720,#34721,
#34722,#34723,#34724,#34725,#34726,#34727,#34728,#34729,#34730,#34731,#34732,
#34733,#34734,#34735,#34736,#34737,#34738,#34739,#34740,#34741,#34742,#34743,
#34744,#34745,#34746,#34747,#34748),(#34749,#34750,#34751,#34752,#34753,
#34754,#34755,#34756,#34757,#34758,#34759,#34760,#34761,#34762,#34763,#34764,
#34765,#34766,#34767,#34768,#34769,#34770,#34771,#34772,#34773,#34774,#34775,
#34776,#34777,#34778,#34779,#34780,#34781,#34782,#34783,#34784,#34785,#34786,
#34787,#34788,#34789,#34790,#34791,#34792,#34793,#34794,#34795,#34796,#34797,
#34798,#34799,#34800,#34801,#34802),(#34803,#34804,#34805,#34806,#34807,
#34808,#34809,#34810,#34811,#34812,#34813,#34814,#34815,#34816,#34817,#34818,
#34819,#34820,#34821,#34822,#34823,#34824,#34825,#34826,#34827,#34828,#34829,
#34830,#34831,#34832,#34833,#34834,#34835,#34836,#34837,#34838,#34839,#34840,
#34841,#34842,#34843,#34844,#34845,#34846,#34847,#34848,#34849,#34850,#34851,
#34852,#34853,#34854,#34855,#34856),(#34857,#34858,#34859,#34860,#34861,
#34862,#34863,#34864,#34865,#34866,#34867,#34868,#34869,#34870,#34871,#34872,
#34873,#34874,#34875,#34876,#34877,#34878,#34879,#34880,#34881,#34882,#34883,
#34884,#34885,#34886,#34887,#34888,#34889,#34890,#34891,#34892,#34893,#34894,
#34895,#34896,#34897,#34898,#34899,#34900,#34901,#34902,#34903,#34904,#34905,
#34906,#34907,#34908,#34909,#34910),(#34911,#34912,#34913,#34914,#34915,
#34916,#34917,#34918,#34919,#34920,#34921,#34922,#34923,#34924,#34925,#34926,
#34927,#34928,#34929,#34930,#34931,#34932,#34933,#34934,#34935,#34936,#34937,
#34938,#34939,#34940,#34941,#34942,#34943,#34944,#34945,#34946,#34947,#34948,
#34949,#34950,#34951,#34952,#34953,#34954,#34955,#34956,#34957,#34958,#34959,
#34960,#34961,#34962,#34963,#34964),(#34965,#34966,#34967,#34968,#34969,
#34970,#34971,#34972,#34973,#34974,#34975,#34976,#34977,#34978,#34979,#34980,
#34981,#34982,#34983,#34984,#34985,#34986,#34987,#34988,#34989,#34990,#34991,
#34992,#34993,#34994,#34995,#34996,#34997,#34998,#34999,#35000,#35001,#35002,
#35003,#35004,#35005,#35006,#35007,#35008,#35009,#35010,#35011,#35012,#35013,
#35014,#35015,#35016,#35017,#35018),(#35019,#35020,#35021,#35022,#35023,
#35024,#35025,#35026,#35027,#35028,#35029,#35030,#35031,#35032,#35033,#35034,
#35035,#35036,#35037,#35038,#35039,#35040,#35041,#35042,#35043,#35044,#35045,
#35046,#35047,#35048,#35049,#35050,#35051,#35052,#35053,#35054,#35055,#35056,
#35057,#35058,#35059,#35060,#35061,#35062,#35063,#35064,#35065,#35066,#35067,
#35068,#35069,#35070,#35071,#35072),(#35073,#35074,#35075,#35076,#35077,
#35078,#35079,#35080,#35081,#35082,#35083,#35084,#35085,#35086,#35087,#35088,
#35089,#35090,#35091,#35092,#35093,#35094,#35095,#35096,#35097,#35098,#35099,
#35100,#35101,#35102,#35103,#35104,#35105,#35106,#35107,#35108,#35109,#35110,
#35111,#35112,#35113,#35114,#35115,#35116,#35117,#35118,#35119,#35120,#35121,
#35122,#35123,#35124,#35125,#35126),(#35127,#35128,#35129,#35130,#35131,
#35132,#35133,#35134,#35135,#35136,#35137,#35138,#35139,#35140,#35141,#35142,
#35143,#35144,#35145,#35146,#35147,#35148,#35149,#35150,#35151,#35152,#35153,
#35154,#35155,#35156,#35157,#35158,#35159,#35160,#35161,#35162,#35163,#35164,
#35165,#35166,#35167,#35168,#35169,#35170,#35171,#35172,#35173,#35174,#35175,
#35176,#35177,#35178,#35179,#35180),(#35181,#35182,#35183,#35184,#35185,
#35186,#35187,#35188,#35189,#35190,#35191,#35192,#35193,#35194,#35195,#35196,
#35197,#35198,#35199,#35200,#35201,#35202,#35203,#35204,#35205,#35206,#35207,
#35208,#35209,#35210,#35211,#35212,#35213,#35214,#35215,#35216,#35217,#35218,
#35219,#35220,#35221,#35222,#35223,#35224,#35225,#35226,#35227,#35228,#35229,
#35230,#35231,#35232,#35233,#35234),(#35235,#35236,#35237,#35238,#35239,
#35240,#35241,#35242,#35243,#35244,#35245,#35246,#35247,#35248,#35249,#35250,
#35251,#35252,#35253,#35254,#35255,#35256,#35257,#35258,#35259,#35260,#35261,
#35262,#35263,#35264,#35265,#35266,#35267,#35268,#35269,#35270,#35271,#35272,
#35273,#35274,#35275,#35276,#35277,#35278,#35279,#35280,#35281,#35282,#35283,
#35284,#35285,#35286,#35287,#35288),(#35289,#35290,#35291,#35292,#35293,
#35294,#35295,#35296,#35297,#35298,#35299,#35300,#35301,#35302,#35303,#35304,
#35305,#35306,#35307,#35308,#35309,#35310,#35311,#35312,#35313,#35314,#35315,
#35316,#35317,#35318,#35319,#35320,#35321,#35322,#35323,#35324,#35325,#35326,
#35327,#35328,#35329,#35330,#35331,#35332,#35333,#35334,#35335,#35336,#35337,
#35338,#35339,#35340,#35341,#35342),(#35343,#35344,#35345,#35346,#35347,
#35348,#35349,#35350,#35351,#35352,#35353,#35354,#35355,#35356,#35357,#35358,
#35359,#35360,#35361,#35362,#35363,#35364,#35365,#35366,#35367,#35368,#35369,
#35370,#35371,#35372,#35373,#35374,#35375,#35376,#35377,#35378,#35379,#35380,
#35381,#35382,#35383,#35384,#35385,#35386,#35387,#35388,#35389,#35390,#35391,
#35392,#35393,#35394,#35395,#35396),(#35397,#35398,#35399,#35400,#35401,
#35402,#35403,#35404,#35405,#35406,#35407,#35408,#35409,#35410,#35411,#35412,
#35413,#35414,#35415,#35416,#35417,#35418,#35419,#35420,#35421,#35422,#35423,
#35424,#35425,#35426,#35427,#35428,#35429,#35430,#35431,#35432,#35433,#35434,
#35435,#35436,#35437,#35438,#35439,#35440,#35441,#35442,#35443,#35444,#35445,
#35446,#35447,#35448,#35449,#35450),(#35451,#35452,#35453,#35454,#35455,
#35456,#35457,#35458,#35459,#35460,#35461,#35462,#35463,#35464,#35465,#35466,
#35467,#35468,#35469,#35470,#35471,#35472,#35473,#35474,#35475,#35476,#35477,
#35478,#35479,#35480,#35481,#35482,#35483,#35484,#35485,#35486,#35487,#35488,
#35489,#35490,#35491,#35492,#35493,#35494,#35495,#35496,#35497,#35498,#35499,
#35500,#35501,#35502,#35503,#35504),(#35505,#35506,#35507,#35508,#35509,
#35510,#35511,#35512,#35513,#35514,#35515,#35516,#35517,#35518,#35519,#35520,
#35521,#35522,#35523,#35524,#35525,#35526,#35527,#35528,#35529,#35530,#35531,
#35532,#35533,#35534,#35535,#35536,#35537,#35538,#35539,#35540,#35541,#35542,
#35543,#35544,#35545,#35546,#35547,#35548,#35549,#35550,#35551,#35552,#35553,
#35554,#35555,#35556,#35557,#35558),(#35559,#35560,#35561,#35562,#35563,
#35564,#35565,#35566,#35567,#35568,#35569,#35570,#35571,#35572,#35573,#35574,
#35575,#35576,#35577,#35578,#35579,#35580,#35581,#35582,#35583,#35584,#35585,
#35586,#35587,#35588,#35589,#35590,#35591,#35592,#35593,#35594,#35595,#35596,
#35597,#35598,#35599,#35600,#35601,#35602,#35603,#35604,#35605,#35606,#35607,
#35608,#35609,#35610,#35611,#35612),(#35613,#35614,#35615,#35616,#35617,
#35618,#35619,#35620,#35621,#35622,#35623,#35624,#35625,#35626,#35627,#35628,
#35629,#35630,#35631,#35632,#35633,#35634,#35635,#35636,#35637,#35638,#35639,
#35640,#35641,#35642,#35643,#35644,#35645,#35646,#35647,#35648,#35649,#35650,
#35651,#35652,#35653,#35654,#35655,#35656,#35657,#35658,#35659,#35660,#35661,
#35662,#35663,#35664,#35665,#35666),(#35667,#35668,#35669,#35670,#35671,
#35672,#35673,#35674,#35675,#35676,#35677,#35678,#35679,#35680,#35681,#35682,
#35683,#35684,#35685,#35686,#35687,#35688,#35689,#35690,#35691,#35692,#35693,
#35694,#35695,#35696,#35697,#35698,#35699,#35700,#35701,#35702,#35703,#35704,
#35705,#35706,#35707,#35708,#35709,#35710,#35711,#35712,#35713,#35714,#35715,
#35716,#35717,#35718,#35719,#35720),(#35721,#35722,#35723,#35724,#35725,
#35726,#35727,#35728,#35729,#35730,#35731,#35732,#35733,#35734,#35735,#35736,
#35737,#35738,#35739,#35740,#35741,#35742,#35743,#35744,#35745,#35746,#35747,
#35748,#35749,#35750,#35751,#35752,#35753,#35754,#35755,#35756,#35757,#35758,
#35759,#35760,#35761,#35762,#35763,#35764,#35765,#35766,#35767,#35768,#35769,
#35770,#35771,#35772,#35773,#35774),(#35775,#35776,#35777,#35778,#35779,
#35780,#35781,#35782,#35783,#35784,#35785,#35786,#35787,#35788,#35789,#35790,
#35791,#35792,#35793,#35794,#35795,#35796,#35797,#35798,#35799,#35800,#35801,
#35802,#35803,#35804,#35805,#35806,#35807,#35808,#35809,#35810,#35811,#35812,
#35813,#35814,#35815,#35816,#35817,#35818,#35819,#35820,#35821,#35822,#35823,
#35824,#35825,#35826,#35827,#35828),(#35829,#35830,#35831,#35832,#35833,
#35834,#35835,#35836,#35837,#35838,#35839,#35840,#35841,#35842,#35843,#35844,
#35845,#35846,#35847,#35848,#35849,#35850,#35851,#35852,#35853,#35854,#35855,
#35856,#35857,#35858,#35859,#35860,#35861,#35862,#35863,#35864,#35865,#35866,
#35867,#35868,#35869,#35870,#35871,#35872,#35873,#35874,#35875,#35876,#35877,
#35878,#35879,#35880,#35881,#35882)),.UNSPECIFIED.,.F.,.F.,.F.,(4,3,3,3,
3,3,3,2,2,2,2,4),(4,3,3,3,3,3,3,3,3,3,3,3,3,3,3,2,2,2,2,4),(-0.01,0.,0.166384002763973,
0.200043514355487,0.333101812640448,0.400072323934008,0.500472422318454,
0.667828884642908,0.667927982169589,0.834482890734559,0.834643736071572,
0.99999999990215),(0.,0.167157083656276,0.174191460919259,0.25514637702534,
0.29512942780803,0.334147528089117,0.384392237472365,0.500992769272865,
0.571140699239784,0.667418852842405,0.667511712013671,0.671156010454595,
0.675688248486018,0.832859978993389,0.833653335891096,0.833768414018777,
0.833810652851698,0.999546262459356,0.999999999996918,1.00999999999673),
 .UNSPECIFIED.);
#256=B_SPLINE_SURFACE_WITH_KNOTS('',3,1,((#36395,#36396,#36397,#36398),
(#36399,#36400,#36401,#36402),(#36403,#36404,#36405,#36406),(#36407,#36408,
#36409,#36410),(#36411,#36412,#36413,#36414),(#36415,#36416,#36417,#36418),
(#36419,#36420,#36421,#36422),(#36423,#36424,#36425,#36426),(#36427,#36428,
#36429,#36430),(#36431,#36432,#36433,#36434),(#36435,#36436,#36437,#36438),
(#36439,#36440,#36441,#36442)),.UNSPECIFIED.,.F.,.F.,.F.,(4,3,2,3,4),(2,
1,1,2),(-0.00114028998203398,0.,0.5,1.,1.00102384459753),(0.0558751001225879,
0.0570163348599441,1.,1.00114002661809),.UNSPECIFIED.);
#257=B_SPLINE_SURFACE_WITH_KNOTS('',3,1,((#36469,#36470,#36471,#36472),
(#36473,#36474,#36475,#36476),(#36477,#36478,#36479,#36480),(#36481,#36482,
#36483,#36484),(#36485,#36486,#36487,#36488),(#36489,#36490,#36491,#36492),
(#36493,#36494,#36495,#36496),(#36497,#36498,#36499,#36500),(#36501,#36502,
#36503,#36504),(#36505,#36506,#36507,#36508),(#36509,#36510,#36511,#36512),
(#36513,#36514,#36515,#36516)),.UNSPECIFIED.,.F.,.F.,.F.,(4,3,2,3,4),(2,
1,1,2),(-0.00042130059479378,0.,0.5,1.,1.00042130059344),(0.0848938236597501,
0.0852822930529455,1.,1.00042026460836),.UNSPECIFIED.);
#258=B_SPLINE_SURFACE_WITH_KNOTS('',3,1,((#36543,#36544,#36545,#36546),
(#36547,#36548,#36549,#36550),(#36551,#36552,#36553,#36554),(#36555,#36556,
#36557,#36558),(#36559,#36560,#36561,#36562),(#36563,#36564,#36565,#36566),
(#36567,#36568,#36569,#36570),(#36571,#36572,#36573,#36574),(#36575,#36576,
#36577,#36578),(#36579,#36580,#36581,#36582),(#36583,#36584,#36585,#36586),
(#36587,#36588,#36589,#36590)),.UNSPECIFIED.,.F.,.F.,.F.,(4,3,2,3,4),(2,
1,1,2),(-0.00102384459755735,0.,0.5,1.,1.00110988099093),(0.0559048734390992,
0.0570163348598889,1.,1.00110970363768),.UNSPECIFIED.);
#259=B_SPLINE_SURFACE_WITH_KNOTS('',3,1,((#36614,#36615,#36616,#36617),
(#36618,#36619,#36620,#36621),(#36622,#36623,#36624,#36625),(#36626,#36627,
#36628,#36629),(#36630,#36631,#36632,#36633),(#36634,#36635,#36636,#36637),
(#36638,#36639,#36640,#36641),(#36642,#36643,#36644,#36645),(#36646,#36647,
#36648,#36649),(#36650,#36651,#36652,#36653),(#36654,#36655,#36656,#36657),
(#36658,#36659,#36660,#36661)),.UNSPECIFIED.,.F.,.F.,.F.,(4,3,2,3,4),(2,
1,1,2),(-0.00102384459755,0.,0.5,1.,1.00110774805047),(0.0559075428418175,
0.0570163348598913,1.,1.00110748137492),.UNSPECIFIED.);
#260=B_SPLINE_SURFACE_WITH_KNOTS('',3,1,((#36688,#36689,#36690,#36691),
(#36692,#36693,#36694,#36695),(#36696,#36697,#36698,#36699),(#36700,#36701,
#36702,#36703),(#36704,#36705,#36706,#36707),(#36708,#36709,#36710,#36711),
(#36712,#36713,#36714,#36715),(#36716,#36717,#36718,#36719),(#36720,#36721,
#36722,#36723),(#36724,#36725,#36726,#36727),(#36728,#36729,#36730,#36731),
(#36732,#36733,#36734,#36735)),.UNSPECIFIED.,.F.,.F.,.F.,(4,3,2,3,4),(2,
1,1,2),(-0.000421300593474756,0.,0.5,1.,1.00042130059483),(0.0848938236597613,
0.0852822930529412,1.,1.00042026460839),.UNSPECIFIED.);
#261=B_SPLINE_SURFACE_WITH_KNOTS('',3,1,((#36762,#36763,#36764,#36765),
(#36766,#36767,#36768,#36769),(#36770,#36771,#36772,#36773),(#36774,#36775,
#36776,#36777),(#36778,#36779,#36780,#36781),(#36782,#36783,#36784,#36785),
(#36786,#36787,#36788,#36789),(#36790,#36791,#36792,#36793),(#36794,#36795,
#36796,#36797),(#36798,#36799,#36800,#36801),(#36802,#36803,#36804,#36805),
(#36806,#36807,#36808,#36809)),.UNSPECIFIED.,.F.,.F.,.F.,(4,3,2,3,4),(2,
1,1,2),(-0.00114028998205408,0.,0.5,1.,1.00102384459758),(0.0558751001225738,
0.0570163348599441,1.,1.00114002661814),.UNSPECIFIED.);
#262=B_SPLINE_SURFACE_WITH_KNOTS('',3,1,((#36833,#36834,#36835,#36836),
(#36837,#36838,#36839,#36840),(#36841,#36842,#36843,#36844),(#36845,#36846,
#36847,#36848),(#36849,#36850,#36851,#36852),(#36853,#36854,#36855,#36856),
(#36857,#36858,#36859,#36860),(#36861,#36862,#36863,#36864),(#36865,#36866,
#36867,#36868),(#36869,#36870,#36871,#36872),(#36873,#36874,#36875,#36876),
(#36877,#36878,#36879,#36880)),.UNSPECIFIED.,.F.,.F.,.F.,(4,3,2,3,4),(2,
1,1,2),(-0.00102363639854971,0.,0.5,1.,1.00044073822443),(0.0558990032510512,
0.0570163348599174,1.,1.00110652324197),.UNSPECIFIED.);
#263=B_SPLINE_SURFACE_WITH_KNOTS('',3,1,((#36908,#36909,#36910,#36911),
(#36912,#36913,#36914,#36915),(#36916,#36917,#36918,#36919),(#36920,#36921,
#36922,#36923),(#36924,#36925,#36926,#36927),(#36928,#36929,#36930,#36931),
(#36932,#36933,#36934,#36935),(#36936,#36937,#36938,#36939),(#36940,#36941,
#36942,#36943),(#36944,#36945,#36946,#36947),(#36948,#36949,#36950,#36951),
(#36952,#36953,#36954,#36955)),.UNSPECIFIED.,.F.,.F.,.F.,(4,3,2,3,4),(2,
1,1,2),(-0.000421300593445888,0.,0.5,1.,1.0004213005948),(0.0848938236598966,
0.0852822930529578,1.,1.00042026460836),.UNSPECIFIED.);
#264=B_SPLINE_SURFACE_WITH_KNOTS('',3,1,((#36982,#36983,#36984,#36985),
(#36986,#36987,#36988,#36989),(#36990,#36991,#36992,#36993),(#36994,#36995,
#36996,#36997),(#36998,#36999,#37000,#37001),(#37002,#37003,#37004,#37005),
(#37006,#37007,#37008,#37009),(#37010,#37011,#37012,#37013),(#37014,#37015,
#37016,#37017),(#37018,#37019,#37020,#37021),(#37022,#37023,#37024,#37025),
(#37026,#37027,#37028,#37029)),.UNSPECIFIED.,.F.,.F.,.F.,(4,3,2,3,4),(2,
1,1,2),(-0.000391510227323989,0.,0.5,1.,1.00030873205263),(0.0567815833000114,
0.0571716035704101,1.,1.00039130192454),.UNSPECIFIED.);
#265=B_SPLINE_SURFACE_WITH_KNOTS('',3,1,((#37048,#37049,#37050,#37051),
(#37052,#37053,#37054,#37055),(#37056,#37057,#37058,#37059),(#37060,#37061,
#37062,#37063),(#37064,#37065,#37066,#37067),(#37068,#37069,#37070,#37071),
(#37072,#37073,#37074,#37075),(#37076,#37077,#37078,#37079),(#37080,#37081,
#37082,#37083),(#37084,#37085,#37086,#37087),(#37088,#37089,#37090,#37091),
(#37092,#37093,#37094,#37095)),.UNSPECIFIED.,.F.,.F.,.F.,(4,3,2,3,4),(2,
1,1,2),(-0.000391510227317498,0.,0.5,1.,1.00030873205267),(0.056781583300018,
0.0571716035704015,1.,1.00039130192453),.UNSPECIFIED.);
#266=B_SPLINE_SURFACE_WITH_KNOTS('',3,1,((#37117,#37118,#37119,#37120),
(#37121,#37122,#37123,#37124),(#37125,#37126,#37127,#37128),(#37129,#37130,
#37131,#37132),(#37133,#37134,#37135,#37136),(#37137,#37138,#37139,#37140),
(#37141,#37142,#37143,#37144),(#37145,#37146,#37147,#37148),(#37149,#37150,
#37151,#37152),(#37153,#37154,#37155,#37156),(#37157,#37158,#37159,#37160),
(#37161,#37162,#37163,#37164)),.UNSPECIFIED.,.F.,.F.,.F.,(4,3,2,3,4),(2,
1,1,2),(-0.000421300594797483,0.,0.5,1.,1.00042130059344),(0.0848938236598713,
0.08528229305296,1.,1.00042026460836),.UNSPECIFIED.);
#267=B_SPLINE_SURFACE_WITH_KNOTS('',3,1,((#37191,#37192,#37193,#37194),
(#37195,#37196,#37197,#37198),(#37199,#37200,#37201,#37202),(#37203,#37204,
#37205,#37206),(#37207,#37208,#37209,#37210),(#37211,#37212,#37213,#37214),
(#37215,#37216,#37217,#37218),(#37219,#37220,#37221,#37222),(#37223,#37224,
#37225,#37226),(#37227,#37228,#37229,#37230),(#37231,#37232,#37233,#37234),
(#37235,#37236,#37237,#37238)),.UNSPECIFIED.,.F.,.F.,.F.,(4,3,2,3,4),(2,
1,1,2),(-0.00102384459763704,0.,0.5,1.,1.00110774805053),(0.0559075428417994,
0.0570163348599251,1.,1.00110748137497),.UNSPECIFIED.);
#268=SHAPE_REPRESENTATION_RELATIONSHIP('SRR','None',#40002,#275);
#269=SHAPE_REPRESENTATION_RELATIONSHIP('SRR','None',#40003,#276);
#270=SHAPE_REPRESENTATION_RELATIONSHIP('SRR','None',#40004,#277);
#271=SHAPE_REPRESENTATION_RELATIONSHIP('SRR','None',#40005,#278);
#272=SHAPE_REPRESENTATION_RELATIONSHIP('SRR','None',#40006,#279);
#273=SHAPE_REPRESENTATION_RELATIONSHIP('SRR','None',#40007,#280);
#274=SHAPE_REPRESENTATION_RELATIONSHIP('SRR','None',#40008,#281);
#275=ADVANCED_BREP_SHAPE_REPRESENTATION('',(#290),#39952);
#276=ADVANCED_BREP_SHAPE_REPRESENTATION('',(#291),#39953);
#277=ADVANCED_BREP_SHAPE_REPRESENTATION('',(#292),#39954);
#278=ADVANCED_BREP_SHAPE_REPRESENTATION('',(#293),#39955);
#279=ADVANCED_BREP_SHAPE_REPRESENTATION('',(#294,#295),#39956);
#280=ADVANCED_BREP_SHAPE_REPRESENTATION('',(#183),#39957);
#281=ADVANCED_BREP_SHAPE_REPRESENTATION('',(#296),#39958);
#282=STYLED_ITEM('',(#40046),#290);
#283=STYLED_ITEM('',(#40046),#291);
#284=STYLED_ITEM('',(#40046),#292);
#285=STYLED_ITEM('',(#40046),#293);
#286=STYLED_ITEM('',(#40046),#294);
#287=STYLED_ITEM('',(#40046),#295);
#288=STYLED_ITEM('',(#40046),#183);
#289=STYLED_ITEM('',(#40046),#296);
#290=MANIFOLD_SOLID_BREP('Body1',#18259);
#291=MANIFOLD_SOLID_BREP('Body1',#18260);
#292=MANIFOLD_SOLID_BREP('Body1',#18261);
#293=MANIFOLD_SOLID_BREP('Body1',#18262);
#294=MANIFOLD_SOLID_BREP('Body1',#18263);
#295=MANIFOLD_SOLID_BREP('Body2',#18264);
#296=MANIFOLD_SOLID_BREP('Body1',#18270);
#297=PLANE('',#18468);
#298=PLANE('',#18469);
#299=PLANE('',#18470);
#300=PLANE('',#18471);
#301=PLANE('',#18472);
#302=PLANE('',#18477);
#303=PLANE('',#18483);
#304=PLANE('',#18485);
#305=PLANE('',#18487);
#306=PLANE('',#18489);
#307=PLANE('',#18490);
#308=PLANE('',#18495);
#309=PLANE('',#18501);
#310=PLANE('',#18503);
#311=PLANE('',#18505);
#312=PLANE('',#18507);
#313=PLANE('',#18508);
#314=PLANE('',#18509);
#315=PLANE('',#18510);
#316=PLANE('',#18511);
#317=PLANE('',#18512);
#318=PLANE('',#18513);
#319=PLANE('',#18514);
#320=PLANE('',#18515);
#321=PLANE('',#18516);
#322=PLANE('',#18517);
#323=PLANE('',#18518);
#324=PLANE('',#18519);
#325=PLANE('',#18520);
#326=PLANE('',#18521);
#327=PLANE('',#18522);
#328=PLANE('',#18523);
#329=PLANE('',#18524);
#330=PLANE('',#18525);
#331=PLANE('',#18526);
#332=PLANE('',#18527);
#333=PLANE('',#18528);
#334=PLANE('',#18529);
#335=PLANE('',#18530);
#336=PLANE('',#18531);
#337=PLANE('',#18532);
#338=PLANE('',#18533);
#339=PLANE('',#18534);
#340=PLANE('',#18535);
#341=PLANE('',#18548);
#342=PLANE('',#18550);
#343=PLANE('',#18554);
#344=PLANE('',#18559);
#345=PLANE('',#18560);
#346=PLANE('',#18580);
#347=PLANE('',#18583);
#348=PLANE('',#18588);
#349=PLANE('',#18593);
#350=PLANE('',#18594);
#351=PLANE('',#18632);
#352=PLANE('',#18666);
#353=PLANE('',#18667);
#354=PLANE('',#18680);
#355=PLANE('',#18684);
#356=PLANE('',#18686);
#357=PLANE('',#18687);
#358=PLANE('',#18688);
#359=PLANE('',#18689);
#360=PLANE('',#18690);
#361=PLANE('',#18691);
#362=PLANE('',#18692);
#363=PLANE('',#18693);
#364=PLANE('',#18694);
#365=PLANE('',#18695);
#366=PLANE('',#18696);
#367=PLANE('',#18697);
#368=PLANE('',#18698);
#369=PLANE('',#18699);
#370=PLANE('',#18700);
#371=PLANE('',#18701);
#372=PLANE('',#18702);
#373=PLANE('',#18703);
#374=PLANE('',#18704);
#375=PLANE('',#18705);
#376=PLANE('',#18706);
#377=PLANE('',#18707);
#378=PLANE('',#18708);
#379=PLANE('',#18709);
#380=PLANE('',#18710);
#381=PLANE('',#18711);
#382=PLANE('',#18712);
#383=PLANE('',#18713);
#384=PLANE('',#18714);
#385=PLANE('',#18715);
#386=PLANE('',#18718);
#387=PLANE('',#18719);
#388=PLANE('',#18720);
#389=PLANE('',#18748);
#390=PLANE('',#18749);
#391=PLANE('',#18765);
#392=PLANE('',#18766);
#393=PLANE('',#18767);
#394=PLANE('',#18768);
#395=PLANE('',#18769);
#396=PLANE('',#18770);
#397=PLANE('',#18771);
#398=PLANE('',#18772);
#399=PLANE('',#18773);
#400=PLANE('',#18774);
#401=PLANE('',#18775);
#402=PLANE('',#18776);
#403=PLANE('',#18777);
#404=PLANE('',#18778);
#405=PLANE('',#18779);
#406=PLANE('',#18780);
#407=PLANE('',#18781);
#408=PLANE('',#18782);
#409=PLANE('',#18783);
#410=PLANE('',#18784);
#411=PLANE('',#18785);
#412=PLANE('',#18786);
#413=PLANE('',#18787);
#414=PLANE('',#18788);
#415=PLANE('',#18789);
#416=PLANE('',#18790);
#417=PLANE('',#18791);
#418=PLANE('',#18792);
#419=PLANE('',#18845);
#420=PLANE('',#18846);
#421=PLANE('',#18850);
#422=PLANE('',#18851);
#423=PLANE('',#18884);
#424=PLANE('',#18885);
#425=PLANE('',#18892);
#426=PLANE('',#18895);
#427=PLANE('',#18896);
#428=PLANE('',#18897);
#429=PLANE('',#18898);
#430=PLANE('',#18899);
#431=PLANE('',#18900);
#432=PLANE('',#18901);
#433=PLANE('',#18902);
#434=PLANE('',#18903);
#435=PLANE('',#18904);
#436=PLANE('',#19106);
#437=PLANE('',#19107);
#438=PLANE('',#19108);
#439=PLANE('',#19109);
#440=PLANE('',#19110);
#441=PLANE('',#19122);
#442=PLANE('',#19123);
#443=PLANE('',#19124);
#444=PLANE('',#19125);
#445=PLANE('',#19126);
#446=PLANE('',#19127);
#447=PLANE('',#19128);
#448=PLANE('',#19129);
#449=PLANE('',#19130);
#450=PLANE('',#19135);
#451=PLANE('',#19137);
#452=PLANE('',#19138);
#453=PLANE('',#19139);
#454=PLANE('',#19140);
#455=PLANE('',#19141);
#456=PLANE('',#19142);
#457=PLANE('',#19143);
#458=PLANE('',#19148);
#459=PLANE('',#19150);
#460=PLANE('',#19151);
#461=PLANE('',#19152);
#462=PLANE('',#19153);
#463=PLANE('',#19154);
#464=PLANE('',#19155);
#465=PLANE('',#19156);
#466=PLANE('',#19161);
#467=PLANE('',#19163);
#468=PLANE('',#19165);
#469=PLANE('',#19166);
#470=PLANE('',#19167);
#471=PLANE('',#19168);
#472=PLANE('',#19169);
#473=PLANE('',#19170);
#474=PLANE('',#19171);
#475=PLANE('',#19175);
#476=PLANE('',#19179);
#477=PLANE('',#19186);
#478=PLANE('',#19193);
#479=PLANE('',#19198);
#480=PLANE('',#19203);
#481=PLANE('',#19205);
#482=PLANE('',#19207);
#483=PLANE('',#19209);
#484=PLANE('',#19211);
#485=PLANE('',#19213);
#486=PLANE('',#19215);
#487=PLANE('',#19217);
#488=PLANE('',#19219);
#489=PLANE('',#19221);
#490=PLANE('',#19223);
#491=PLANE('',#19225);
#492=PLANE('',#19229);
#493=PLANE('',#19232);
#494=PLANE('',#19234);
#495=PLANE('',#19237);
#496=PLANE('',#19239);
#497=PLANE('',#19242);
#498=PLANE('',#19243);
#499=PLANE('',#19246);
#500=PLANE('',#19247);
#501=PLANE('',#19250);
#502=PLANE('',#19251);
#503=PLANE('',#19254);
#504=PLANE('',#19255);
#505=PLANE('',#19263);
#506=PLANE('',#19268);
#507=PLANE('',#19271);
#508=PLANE('',#19274);
#509=PLANE('',#19277);
#510=PLANE('',#19278);
#511=PLANE('',#19280);
#512=PLANE('',#19282);
#513=PLANE('',#19284);
#514=PLANE('',#19286);
#515=PLANE('',#19288);
#516=PLANE('',#19289);
#517=PLANE('',#19290);
#518=PLANE('',#19292);
#519=PLANE('',#19294);
#520=PLANE('',#19296);
#521=PLANE('',#19298);
#522=PLANE('',#19301);
#523=PLANE('',#19303);
#524=PLANE('',#19306);
#525=PLANE('',#19308);
#526=PLANE('',#19310);
#527=PLANE('',#19345);
#528=PLANE('',#19346);
#529=PLANE('',#19349);
#530=PLANE('',#19356);
#531=PLANE('',#19371);
#532=PLANE('',#19383);
#533=PLANE('',#19384);
#534=PLANE('',#19391);
#535=PLANE('',#19392);
#536=PLANE('',#19393);
#537=PLANE('',#19400);
#538=PLANE('',#19401);
#539=PLANE('',#19402);
#540=PLANE('',#19407);
#541=PLANE('',#19408);
#542=PLANE('',#19409);
#543=PLANE('',#19416);
#544=PLANE('',#19417);
#545=PLANE('',#19418);
#546=PLANE('',#19423);
#547=PLANE('',#19424);
#548=PLANE('',#19425);
#549=PLANE('',#19426);
#550=PLANE('',#19427);
#551=PLANE('',#19428);
#552=PLANE('',#19429);
#553=PLANE('',#19430);
#554=PLANE('',#19431);
#555=PLANE('',#19432);
#556=PLANE('',#19433);
#557=PLANE('',#19434);
#558=PLANE('',#19441);
#559=PLANE('',#19442);
#560=PLANE('',#19455);
#561=PLANE('',#19459);
#562=PLANE('',#19460);
#563=PLANE('',#19461);
#564=PLANE('',#19462);
#565=PLANE('',#19463);
#566=PLANE('',#19469);
#567=PLANE('',#19470);
#568=PLANE('',#19471);
#569=PLANE('',#19473);
#570=PLANE('',#19474);
#571=PLANE('',#19475);
#572=PLANE('',#19476);
#573=PLANE('',#19477);
#574=PLANE('',#19482);
#575=PLANE('',#19483);
#576=PLANE('',#19484);
#577=PLANE('',#19485);
#578=PLANE('',#19491);
#579=PLANE('',#19492);
#580=PLANE('',#19496);
#581=PLANE('',#19497);
#582=PLANE('',#19498);
#583=PLANE('',#19501);
#584=PLANE('',#19502);
#585=PLANE('',#19503);
#586=PLANE('',#19504);
#587=PLANE('',#19508);
#588=PLANE('',#19511);
#589=PLANE('',#19512);
#590=PLANE('',#19513);
#591=PLANE('',#19516);
#592=PLANE('',#19517);
#593=PLANE('',#19521);
#594=PLANE('',#19524);
#595=PLANE('',#19525);
#596=PLANE('',#19526);
#597=PLANE('',#19529);
#598=PLANE('',#19530);
#599=PLANE('',#19534);
#600=PLANE('',#19537);
#601=PLANE('',#19538);
#602=PLANE('',#19539);
#603=PLANE('',#19542);
#604=PLANE('',#19543);
#605=PLANE('',#19547);
#606=PLANE('',#19550);
#607=PLANE('',#19551);
#608=PLANE('',#19552);
#609=PLANE('',#19555);
#610=PLANE('',#19556);
#611=PLANE('',#19557);
#612=PLANE('',#19558);
#613=PLANE('',#19559);
#614=PLANE('',#19560);
#615=PLANE('',#19561);
#616=PLANE('',#19562);
#617=PLANE('',#19563);
#618=PLANE('',#19564);
#619=PLANE('',#19565);
#620=PLANE('',#19566);
#621=PLANE('',#19567);
#622=PLANE('',#19568);
#623=PLANE('',#19569);
#624=PLANE('',#19570);
#625=PLANE('',#19571);
#626=PLANE('',#19572);
#627=PLANE('',#19573);
#628=PLANE('',#19577);
#629=PLANE('',#19578);
#630=PLANE('',#19580);
#631=PLANE('',#19581);
#632=PLANE('',#19584);
#633=PLANE('',#19585);
#634=PLANE('',#19586);
#635=PLANE('',#19587);
#636=PLANE('',#19590);
#637=PLANE('',#19591);
#638=PLANE('',#19593);
#639=PLANE('',#19594);
#640=PLANE('',#19598);
#641=PLANE('',#19599);
#642=PLANE('',#19601);
#643=PLANE('',#19602);
#644=PLANE('',#19603);
#645=PLANE('',#19605);
#646=PLANE('',#19607);
#647=PLANE('',#19609);
#648=PLANE('',#19610);
#649=PLANE('',#19612);
#650=PLANE('',#19614);
#651=PLANE('',#19616);
#652=PLANE('',#19618);
#653=PLANE('',#19619);
#654=PLANE('',#19622);
#655=PLANE('',#19625);
#656=PLANE('',#19626);
#657=PLANE('',#19628);
#658=PLANE('',#19629);
#659=PLANE('',#19630);
#660=PLANE('',#19631);
#661=PLANE('',#19632);
#662=PLANE('',#19633);
#663=PLANE('',#19636);
#664=PLANE('',#19639);
#665=PLANE('',#19640);
#666=PLANE('',#19641);
#667=PLANE('',#19642);
#668=PLANE('',#19643);
#669=PLANE('',#19647);
#670=PLANE('',#19648);
#671=PLANE('',#19649);
#672=PLANE('',#19650);
#673=PLANE('',#19651);
#674=PLANE('',#19653);
#675=PLANE('',#19654);
#676=PLANE('',#19656);
#677=PLANE('',#19658);
#678=PLANE('',#19659);
#679=PLANE('',#19661);
#680=PLANE('',#19664);
#681=PLANE('',#19666);
#682=PLANE('',#19667);
#683=PLANE('',#19669);
#684=PLANE('',#19671);
#685=PLANE('',#19672);
#686=PLANE('',#19674);
#687=PLANE('',#19675);
#688=PLANE('',#19676);
#689=PLANE('',#19677);
#690=PLANE('',#19678);
#691=PLANE('',#19679);
#692=PLANE('',#19680);
#693=PLANE('',#19684);
#694=PLANE('',#19687);
#695=PLANE('',#19690);
#696=PLANE('',#19691);
#697=PLANE('',#19692);
#698=PLANE('',#19693);
#699=PLANE('',#19694);
#700=PLANE('',#19695);
#701=PLANE('',#19696);
#702=PLANE('',#19697);
#703=PLANE('',#19698);
#704=PLANE('',#19699);
#705=PLANE('',#19700);
#706=PLANE('',#19701);
#707=PLANE('',#19702);
#708=PLANE('',#19703);
#709=PLANE('',#19704);
#710=PLANE('',#19709);
#711=PLANE('',#19711);
#712=PLANE('',#19712);
#713=PLANE('',#19713);
#714=PLANE('',#19714);
#715=PLANE('',#19715);
#716=PLANE('',#19716);
#717=PLANE('',#19720);
#718=PLANE('',#19722);
#719=PLANE('',#19723);
#720=PLANE('',#19724);
#721=PLANE('',#19725);
#722=PLANE('',#19726);
#723=PLANE('',#19727);
#724=PLANE('',#19732);
#725=PLANE('',#19736);
#726=PLANE('',#19739);
#727=PLANE('',#19744);
#728=PLANE('',#19745);
#729=PLANE('',#19747);
#730=PLANE('',#19750);
#731=PLANE('',#19754);
#732=PLANE('',#19758);
#733=PLANE('',#19759);
#734=PLANE('',#19760);
#735=PLANE('',#19761);
#736=PLANE('',#19762);
#737=PLANE('',#19763);
#738=PLANE('',#19764);
#739=PLANE('',#19768);
#740=PLANE('',#19770);
#741=PLANE('',#19771);
#742=PLANE('',#19772);
#743=PLANE('',#19773);
#744=PLANE('',#19774);
#745=PLANE('',#19775);
#746=PLANE('',#19776);
#747=PLANE('',#19777);
#748=PLANE('',#19778);
#749=PLANE('',#19779);
#750=PLANE('',#19780);
#751=PLANE('',#19781);
#752=PLANE('',#19782);
#753=PLANE('',#19783);
#754=PLANE('',#19784);
#755=PLANE('',#19785);
#756=PLANE('',#19786);
#757=PLANE('',#19787);
#758=PLANE('',#19788);
#759=PLANE('',#19789);
#760=PLANE('',#19790);
#761=PLANE('',#19791);
#762=PLANE('',#19792);
#763=PLANE('',#19793);
#764=PLANE('',#19794);
#765=PLANE('',#19795);
#766=PLANE('',#19797);
#767=PLANE('',#19798);
#768=PLANE('',#19799);
#769=PLANE('',#19801);
#770=PLANE('',#19802);
#771=PLANE('',#19803);
#772=PLANE('',#19805);
#773=PLANE('',#19808);
#774=PLANE('',#19812);
#775=PLANE('',#19815);
#776=PLANE('',#19817);
#777=PLANE('',#19821);
#778=PLANE('',#19823);
#779=PLANE('',#19824);
#780=PLANE('',#19825);
#781=PLANE('',#19826);
#782=PLANE('',#19827);
#783=PLANE('',#19828);
#784=PLANE('',#19829);
#785=PLANE('',#19830);
#786=PLANE('',#19831);
#787=PLANE('',#19832);
#788=PLANE('',#19833);
#789=PLANE('',#19834);
#790=PLANE('',#19835);
#791=PLANE('',#19836);
#792=PLANE('',#19837);
#793=PLANE('',#19838);
#794=PLANE('',#19839);
#795=PLANE('',#19840);
#796=PLANE('',#19842);
#797=PLANE('',#19844);
#798=PLANE('',#19845);
#799=PLANE('',#19849);
#800=PLANE('',#19853);
#801=PLANE('',#19854);
#802=PLANE('',#19855);
#803=PLANE('',#19857);
#804=PLANE('',#19859);
#805=PLANE('',#19865);
#806=PLANE('',#19872);
#807=PLANE('',#19874);
#808=PLANE('',#19875);
#809=PLANE('',#19876);
#810=PLANE('',#19877);
#811=PLANE('',#19878);
#812=PLANE('',#19879);
#813=PLANE('',#19880);
#814=PLANE('',#19881);
#815=PLANE('',#19882);
#816=PLANE('',#19883);
#817=PLANE('',#19884);
#818=PLANE('',#19885);
#819=PLANE('',#19886);
#820=PLANE('',#19887);
#821=PLANE('',#19888);
#822=PLANE('',#19895);
#823=PLANE('',#19896);
#824=PLANE('',#19897);
#825=PLANE('',#19898);
#826=PLANE('',#19899);
#827=PLANE('',#19900);
#828=PLANE('',#19901);
#829=PLANE('',#19912);
#830=PLANE('',#19913);
#831=PLANE('',#19914);
#832=PLANE('',#19915);
#833=PLANE('',#19916);
#834=PLANE('',#19917);
#835=PLANE('',#19918);
#836=PLANE('',#19919);
#837=PLANE('',#19920);
#838=PLANE('',#19921);
#839=PLANE('',#19922);
#840=PLANE('',#19923);
#841=PLANE('',#19924);
#842=PLANE('',#19925);
#843=PLANE('',#19926);
#844=PLANE('',#19927);
#845=PLANE('',#19928);
#846=PLANE('',#19929);
#847=PLANE('',#19930);
#848=PLANE('',#19931);
#849=PLANE('',#19932);
#850=PLANE('',#19933);
#851=PLANE('',#19934);
#852=PLANE('',#19935);
#853=PLANE('',#19936);
#854=PLANE('',#19937);
#855=PLANE('',#19938);
#856=PLANE('',#19939);
#857=PLANE('',#19940);
#858=PLANE('',#19941);
#859=PLANE('',#19942);
#860=PLANE('',#19943);
#861=PLANE('',#19962);
#862=PLANE('',#19963);
#863=PLANE('',#19964);
#864=PLANE('',#19965);
#865=PLANE('',#19966);
#866=PLANE('',#19967);
#867=PLANE('',#19968);
#868=PLANE('',#19969);
#869=PLANE('',#19970);
#870=PLANE('',#19983);
#871=PLANE('',#19984);
#872=PLANE('',#19985);
#873=PLANE('',#19986);
#874=PLANE('',#19987);
#875=PLANE('',#19988);
#876=FACE_BOUND('',#5847,.T.);
#877=FACE_BOUND('',#5848,.T.);
#878=FACE_BOUND('',#5851,.T.);
#879=FACE_BOUND('',#5852,.T.);
#880=FACE_BOUND('',#5854,.T.);
#881=FACE_BOUND('',#5856,.T.);
#882=FACE_BOUND('',#5857,.T.);
#883=FACE_BOUND('',#5858,.T.);
#884=FACE_BOUND('',#5859,.T.);
#885=FACE_BOUND('',#5860,.T.);
#886=FACE_BOUND('',#5861,.T.);
#887=FACE_BOUND('',#5862,.T.);
#888=FACE_BOUND('',#5863,.T.);
#889=FACE_BOUND('',#5864,.T.);
#890=FACE_BOUND('',#5865,.T.);
#891=FACE_BOUND('',#5866,.T.);
#892=FACE_BOUND('',#5867,.T.);
#893=FACE_BOUND('',#5868,.T.);
#894=FACE_BOUND('',#5869,.T.);
#895=FACE_BOUND('',#5870,.T.);
#896=FACE_BOUND('',#5871,.T.);
#897=FACE_BOUND('',#5873,.T.);
#898=FACE_BOUND('',#5874,.T.);
#899=FACE_BOUND('',#5875,.T.);
#900=FACE_BOUND('',#5876,.T.);
#901=FACE_BOUND('',#5877,.T.);
#902=FACE_BOUND('',#5878,.T.);
#903=FACE_BOUND('',#5879,.T.);
#904=FACE_BOUND('',#5880,.T.);
#905=FACE_BOUND('',#5881,.T.);
#906=FACE_BOUND('',#5882,.T.);
#907=FACE_BOUND('',#5883,.T.);
#908=FACE_BOUND('',#5884,.T.);
#909=FACE_BOUND('',#5885,.T.);
#910=FACE_BOUND('',#5886,.T.);
#911=FACE_BOUND('',#5887,.T.);
#912=FACE_BOUND('',#5888,.T.);
#913=FACE_BOUND('',#5890,.T.);
#914=FACE_BOUND('',#5892,.T.);
#915=FACE_BOUND('',#5893,.T.);
#916=FACE_BOUND('',#5894,.T.);
#917=FACE_BOUND('',#5895,.T.);
#918=FACE_BOUND('',#5896,.T.);
#919=FACE_BOUND('',#5898,.T.);
#920=FACE_BOUND('',#5899,.T.);
#921=FACE_BOUND('',#5900,.T.);
#922=FACE_BOUND('',#5901,.T.);
#923=FACE_BOUND('',#5902,.T.);
#924=FACE_BOUND('',#5912,.T.);
#925=FACE_BOUND('',#5913,.T.);
#926=FACE_BOUND('',#5914,.T.);
#927=FACE_BOUND('',#5915,.T.);
#928=FACE_BOUND('',#5916,.T.);
#929=FACE_BOUND('',#5918,.T.);
#930=FACE_BOUND('',#5919,.T.);
#931=FACE_BOUND('',#5920,.T.);
#932=FACE_BOUND('',#5921,.T.);
#933=FACE_BOUND('',#5922,.T.);
#934=FACE_BOUND('',#5932,.T.);
#935=FACE_BOUND('',#5965,.T.);
#936=FACE_BOUND('',#5967,.T.);
#937=FACE_BOUND('',#5986,.T.);
#938=FACE_BOUND('',#5988,.T.);
#939=FACE_BOUND('',#5994,.T.);
#940=FACE_BOUND('',#5995,.T.);
#941=FACE_BOUND('',#5997,.T.);
#942=FACE_BOUND('',#5998,.T.);
#943=FACE_BOUND('',#6010,.T.);
#944=FACE_BOUND('',#6012,.T.);
#945=FACE_BOUND('',#6013,.T.);
#946=FACE_BOUND('',#6014,.T.);
#947=FACE_BOUND('',#6015,.T.);
#948=FACE_BOUND('',#6016,.T.);
#949=FACE_BOUND('',#6018,.T.);
#950=FACE_BOUND('',#6028,.T.);
#951=FACE_BOUND('',#6030,.T.);
#952=FACE_BOUND('',#6038,.T.);
#953=FACE_BOUND('',#6040,.T.);
#954=FACE_BOUND('',#6088,.T.);
#955=FACE_BOUND('',#6090,.T.);
#956=FACE_BOUND('',#6112,.T.);
#957=FACE_BOUND('',#6113,.T.);
#958=FACE_BOUND('',#6114,.T.);
#959=FACE_BOUND('',#6115,.T.);
#960=FACE_BOUND('',#6117,.T.);
#961=FACE_BOUND('',#6118,.T.);
#962=FACE_BOUND('',#6119,.T.);
#963=FACE_BOUND('',#6120,.T.);
#964=FACE_BOUND('',#6153,.T.);
#965=FACE_BOUND('',#6154,.T.);
#966=FACE_BOUND('',#6155,.T.);
#967=FACE_BOUND('',#6156,.T.);
#968=FACE_BOUND('',#6157,.T.);
#969=FACE_BOUND('',#6158,.T.);
#970=FACE_BOUND('',#6159,.T.);
#971=FACE_BOUND('',#6160,.T.);
#972=FACE_BOUND('',#6161,.T.);
#973=FACE_BOUND('',#6162,.T.);
#974=FACE_BOUND('',#6163,.T.);
#975=FACE_BOUND('',#6164,.T.);
#976=FACE_BOUND('',#6165,.T.);
#977=FACE_BOUND('',#6166,.T.);
#978=FACE_BOUND('',#6167,.T.);
#979=FACE_BOUND('',#6168,.T.);
#980=FACE_BOUND('',#6170,.T.);
#981=FACE_BOUND('',#6171,.T.);
#982=FACE_BOUND('',#6172,.T.);
#983=FACE_BOUND('',#6173,.T.);
#984=FACE_BOUND('',#6174,.T.);
#985=FACE_BOUND('',#6175,.T.);
#986=FACE_BOUND('',#6176,.T.);
#987=FACE_BOUND('',#6177,.T.);
#988=FACE_BOUND('',#6178,.T.);
#989=FACE_BOUND('',#6179,.T.);
#990=FACE_BOUND('',#6180,.T.);
#991=FACE_BOUND('',#6181,.T.);
#992=FACE_BOUND('',#6182,.T.);
#993=FACE_BOUND('',#6183,.T.);
#994=FACE_BOUND('',#6184,.T.);
#995=FACE_BOUND('',#6185,.T.);
#996=FACE_BOUND('',#6199,.T.);
#997=FACE_BOUND('',#6201,.T.);
#998=FACE_BOUND('',#6205,.T.);
#999=FACE_BOUND('',#6248,.T.);
#1000=FACE_BOUND('',#6364,.T.);
#1001=FACE_BOUND('',#6367,.T.);
#1002=FACE_BOUND('',#6369,.T.);
#1003=FACE_BOUND('',#6372,.T.);
#1004=FACE_BOUND('',#6386,.T.);
#1005=FACE_BOUND('',#6388,.T.);
#1006=FACE_BOUND('',#6390,.T.);
#1007=FACE_BOUND('',#6392,.T.);
#1008=FACE_BOUND('',#6466,.T.);
#1009=FACE_BOUND('',#6484,.T.);
#1010=FACE_BOUND('',#6485,.T.);
#1011=FACE_BOUND('',#6505,.T.);
#1012=FACE_BOUND('',#6550,.T.);
#1013=FACE_BOUND('',#6557,.T.);
#1014=FACE_BOUND('',#6560,.T.);
#1015=FACE_BOUND('',#6562,.T.);
#1016=FACE_BOUND('',#6569,.T.);
#1017=FACE_BOUND('',#6579,.T.);
#1018=FACE_BOUND('',#6585,.T.);
#1019=FACE_BOUND('',#6588,.T.);
#1020=FACE_BOUND('',#6594,.T.);
#1021=FACE_BOUND('',#6596,.T.);
#1022=FACE_BOUND('',#6606,.T.);
#1023=FACE_BOUND('',#6616,.T.);
#1024=FACE_BOUND('',#6626,.T.);
#1025=FACE_BOUND('',#6642,.T.);
#1026=FACE_BOUND('',#6644,.T.);
#1027=FACE_BOUND('',#6670,.T.);
#1028=FACE_BOUND('',#6688,.T.);
#1029=FACE_BOUND('',#6692,.T.);
#1030=FACE_BOUND('',#6704,.T.);
#1031=FACE_BOUND('',#6706,.T.);
#1032=FACE_BOUND('',#6708,.T.);
#1033=FACE_BOUND('',#6710,.T.);
#1034=FACE_BOUND('',#6712,.T.);
#1035=FACE_BOUND('',#6740,.T.);
#1036=FACE_BOUND('',#6748,.T.);
#1037=FACE_BOUND('',#6781,.T.);
#1038=FACE_BOUND('',#6818,.T.);
#1039=FACE_BOUND('',#6821,.T.);
#1040=FACE_BOUND('',#6822,.T.);
#1041=FACE_BOUND('',#6823,.T.);
#1042=FACE_BOUND('',#6824,.T.);
#1043=FACE_BOUND('',#6825,.T.);
#1044=FACE_BOUND('',#6843,.T.);
#1045=FACE_BOUND('',#6846,.T.);
#1046=FACE_BOUND('',#6849,.T.);
#1047=FACE_BOUND('',#6857,.T.);
#1048=FACE_BOUND('',#6860,.T.);
#1049=FACE_BOUND('',#6862,.T.);
#1050=FACE_BOUND('',#6877,.T.);
#1051=FACE_BOUND('',#6894,.T.);
#1052=FACE_BOUND('',#6898,.T.);
#1053=FACE_BOUND('',#6906,.T.);
#1054=FACE_BOUND('',#6930,.T.);
#1055=FACE_BOUND('',#6938,.T.);
#1056=FACE_BOUND('',#6943,.T.);
#1057=FACE_BOUND('',#6949,.T.);
#1058=FACE_BOUND('',#6953,.T.);
#1059=FACE_BOUND('',#6954,.T.);
#1060=FACE_BOUND('',#6967,.T.);
#1061=FACE_BOUND('',#6968,.T.);
#1062=FACE_BOUND('',#6969,.T.);
#1063=FACE_BOUND('',#6970,.T.);
#1064=FACE_BOUND('',#6976,.T.);
#1065=B_SPLINE_CURVE_WITH_KNOTS('',3,(#25049,#25050,#25051,#25052,#25053,
#25054,#25055,#25056,#25057,#25058,#25059,#25060,#25061,#25062,#25063,#25064,
#25065,#25066,#25067,#25068,#25069,#25070,#25071,#25072,#25073,#25074,#25075,
#25076,#25077,#25078,#25079,#25080,#25081,#25082,#25083,#25084,#25085,#25086,
#25087,#25088,#25089,#25090,#25091,#25092,#25093,#25094,#25095,#25096,#25097,
#25098,#25099,#25100,#25101,#25102,#25103,#25104,#25105,#25106,#25107,#25108,
#25109,#25110),.UNSPECIFIED.,.T.,.F.,(4,2,2,2,2,2,2,2,2,2,2,2,2,2,2,2,2,
2,2,2,2,2,2,2,2,2,2,2,2,2,4),(-19.6507571622069,-19.4050828429219,-19.1594085236369,
-18.6130728294486,-18.0667371352602,-17.0841171850828,-16.1014972349054,
-15.118877284728,-14.1362573345506,-12.6705405954362,-11.937682225879,-11.2048238563218,
-10.8599625375172,-10.5151012187126,-10.170239899908,-9.82537858110344,
-9.48051726229887,-9.13565594349429,-8.79079462468971,-8.44593330588513,
-7.71307493632793,-6.98021656677073,-5.51449982765633,-4.53187987747891,
-3.54925992730149,-2.56663997712407,-1.58402002694665,-1.03768433275833,
-0.491348638570005,-0.245674319285003,0.),.UNSPECIFIED.);
#1066=B_SPLINE_CURVE_WITH_KNOTS('',3,(#25116,#25117,#25118,#25119,#25120,
#25121,#25122,#25123,#25124,#25125,#25126,#25127,#25128,#25129,#25130,#25131,
#25132,#25133,#25134,#25135,#25136,#25137,#25138,#25139,#25140,#25141,#25142,
#25143,#25144,#25145,#25146,#25147,#25148,#25149,#25150,#25151,#25152,#25153,
#25154,#25155,#25156,#25157,#25158,#25159,#25160,#25161,#25162,#25163,#25164,
#25165,#25166,#25167,#25168,#25169,#25170,#25171,#25172,#25173,#25174,#25175,
#25176,#25177),.UNSPECIFIED.,.T.,.F.,(4,2,2,2,2,2,2,2,2,2,2,2,2,2,2,2,2,
2,2,2,2,2,2,2,2,2,2,2,2,2,4),(-19.6507571622069,-19.3058958434024,-18.9610345245978,
-18.6161732057932,-18.2713118869886,-17.5384535174314,-16.8055951478742,
-15.3398784087598,-14.3572584585824,-13.374638508405,-12.3920185582275,
-11.4093986080501,-10.8630629138618,-10.3167272196735,-10.0710529003885,
-9.82537858110347,-9.57970426181847,-9.33402994253347,-8.78769424834514,
-8.24135855415682,-7.25873860397939,-6.27611865380197,-5.29349870362454,
-4.31087875344711,-2.84516201433271,-2.11230364477551,-1.37944527521831,
-1.03458395641373,-0.689722637609155,-0.344861318804578,0.),
 .UNSPECIFIED.);
#1067=B_SPLINE_CURVE_WITH_KNOTS('',3,(#25183,#25184,#25185,#25186,#25187,
#25188,#25189,#25190,#25191,#25192,#25193,#25194,#25195,#25196,#25197,#25198,
#25199,#25200,#25201,#25202,#25203,#25204,#25205,#25206,#25207,#25208,#25209,
#25210,#25211,#25212,#25213,#25214,#25215,#25216,#25217,#25218,#25219,#25220,
#25221,#25222,#25223,#25224,#25225,#25226,#25227,#25228,#25229,#25230,#25231,
#25232,#25233,#25234,#25235,#25236,#25237,#25238,#25239,#25240,#25241,#25242,
#25243,#25244,#25245,#25246,#25247,#25248),.UNSPECIFIED.,.T.,.F.,(4,2,2,
2,2,2,2,2,2,2,2,2,2,2,2,2,2,2,2,2,2,2,2,2,2,2,2,2,2,2,2,2,4),(-18.9027433334398,
-18.6305373935122,-18.3583314535845,-17.8139195737293,-17.1230429609855,
-16.4321663482417,-15.050413122754,-14.0219604634627,-12.9935078041713,
-11.9650551448799,-10.9366024855886,-10.3754064287965,-10.0948084004005,
-9.81421037200448,-9.63279101936218,-9.54208134304104,-9.45137166671989,
-9.36066199039874,-9.26995231407759,-9.08853296143529,-8.80793493303927,
-8.52733690464326,-7.96614084785122,-6.93768818855985,-5.90923552926848,
-4.88078286997711,-3.85233021068574,-2.47057698519811,-1.7797003724543,
-1.08882375971048,-0.54441187985524,-0.27220593992762,0.),.UNSPECIFIED.);
#1068=B_SPLINE_CURVE_WITH_KNOTS('',3,(#25254,#25255,#25256,#25257,#25258,
#25259,#25260,#25261,#25262,#25263,#25264,#25265,#25266,#25267,#25268,#25269,
#25270,#25271,#25272,#25273,#25274,#25275,#25276,#25277,#25278,#25279,#25280,
#25281,#25282,#25283,#25284,#25285,#25286,#25287,#25288,#25289,#25290,#25291,
#25292,#25293,#25294,#25295,#25296,#25297,#25298,#25299,#25300,#25301,#25302,
#25303,#25304,#25305,#25306,#25307,#25308,#25309,#25310,#25311,#25312,#25313,
#25314,#25315,#25316,#25317,#25318,#25319),.UNSPECIFIED.,.T.,.F.,(4,2,2,
2,2,2,2,2,2,2,2,2,2,2,2,2,2,2,2,2,2,2,2,2,2,2,2,2,2,2,2,2,4),(-18.9027433334398,
-18.8120336571186,-18.7213239807975,-18.5399046281552,-18.2593065997592,
-17.9787085713631,-17.4175125145711,-16.3890598552797,-15.3606071959884,
-14.332154536697,-13.3037018774056,-11.921948651918,-11.2310720391742,-10.5401954264304,
-9.99578354657513,-9.72357760664751,-9.45137166671989,-9.17916572679227,
-8.90695978686465,-8.36254790700941,-7.67167129426559,-6.98079468152178,
-5.59904145603415,-4.57058879674278,-3.54213613745141,-2.51368347816004,
-1.48523081886867,-0.924034762076629,-0.643436733680611,-0.362838705284593,
-0.181419352642297,-0.0907096763211483,0.),.UNSPECIFIED.);
#1069=B_SPLINE_CURVE_WITH_KNOTS('',3,(#25647,#25648,#25649,#25650,#25651,
#25652),.UNSPECIFIED.,.F.,.F.,(4,2,4),(0.376702875081531,0.565054310328979,
0.753405745576428),.UNSPECIFIED.);
#1070=B_SPLINE_CURVE_WITH_KNOTS('',3,(#25654,#25655,#25656,#25657,#25658,
#25659),.UNSPECIFIED.,.F.,.F.,(4,2,4),(0.000204272915071079,0.188351437540765,
0.376680075941862),.UNSPECIFIED.);
#1071=B_SPLINE_CURVE_WITH_KNOTS('',3,(#25661,#25662,#25663,#25664,#25665,
#25666,#25667,#25668,#25669),.UNSPECIFIED.,.F.,.F.,(4,2,3,4),(2.63715317341441,
2.82527154476495,3.01362298230571,3.01382725522078),.UNSPECIFIED.);
#1072=B_SPLINE_CURVE_WITH_KNOTS('',3,(#25671,#25672,#25673,#25674,#25675,
#25676,#25677,#25678),.UNSPECIFIED.,.F.,.F.,(4,2,2,4),(2.26024327400092,
2.44856867197673,2.63692010722418,2.63715317341441),.UNSPECIFIED.);
#1073=B_SPLINE_CURVE_WITH_KNOTS('',3,(#25680,#25681,#25682,#25683,#25684,
#25685),.UNSPECIFIED.,.F.,.F.,(4,2,4),(1.88394027377768,2.07186580148184,
2.26021723672928),.UNSPECIFIED.);
#1074=B_SPLINE_CURVE_WITH_KNOTS('',3,(#25687,#25688,#25689,#25690,#25691,
#25692,#25693,#25694),.UNSPECIFIED.,.F.,.F.,(4,2,2,4),(1.5073284029247,
1.69516292869362,1.88351436623439,1.88394027377768),.UNSPECIFIED.);
#1075=B_SPLINE_CURVE_WITH_KNOTS('',3,(#25696,#25697,#25698,#25699,#25700,
#25701,#25702,#25703),.UNSPECIFIED.,.F.,.F.,(4,2,2,4),(1.13044830756701,
1.31846005361209,1.50681149115286,1.5073284029247),.UNSPECIFIED.);
#1076=B_SPLINE_CURVE_WITH_KNOTS('',3,(#25704,#25705,#25706,#25707,#25708,
#25709,#25710,#25711),.UNSPECIFIED.,.F.,.F.,(4,2,2,4),(0.753405745576428,
0.941757180823877,1.13010861607133,1.13044830756701),.UNSPECIFIED.);
#1077=B_SPLINE_CURVE_WITH_KNOTS('',3,(#25741,#25742,#25743,#25744,#25745,
#25746,#25747,#25748,#25749,#25750,#25751,#25752,#25753,#25754,#25755,#25756,
#25757,#25758,#25759,#25760,#25761,#25762,#25763,#25764,#25765,#25766,#25767,
#25768,#25769,#25770,#25771,#25772,#25773,#25774,#25775,#25776,#25777,#25778,
#25779,#25780,#25781,#25782,#25783,#25784,#25785,#25786,#25787,#25788,#25789,
#25790,#25791,#25792,#25793,#25794,#25795,#25796,#25797,#25798),
 .UNSPECIFIED.,.F.,.F.,(4,3,3,3,3,3,3,3,3,3,3,3,3,3,3,3,3,3,3,4),(0.124997637865204,
0.125004803698825,0.125015258789063,0.134771361364135,0.14467040638079,
0.154662369733195,0.164672368730329,0.174624579474319,0.184411644454489,
0.187522888183594,0.197283569985428,0.207159003809817,0.217118120942224,
0.21877670288086,0.227396265155205,0.2359533648241,0.244350344839939,0.250020612142817,
0.250030517578125,0.250040203921046),.UNSPECIFIED.);
#1078=B_SPLINE_CURVE_WITH_KNOTS('',3,(#25800,#25801,#25802,#25803,#25804,
#25805,#25806,#25807,#25808,#25809,#25810,#25811,#25812,#25813,#25814,#25815,
#25816,#25817,#25818,#25819,#25820,#25821,#25822,#25823,#25824,#25825,#25826,
#25827,#25828,#25829,#25830,#25831,#25832,#25833,#25834,#25835,#25836),
 .UNSPECIFIED.,.F.,.F.,(4,3,3,3,3,3,3,3,3,3,3,3,4),(0.,0.0100788585654741,
0.0205391817562645,0.0308655410000762,0.04118079735384,0.0514218014928902,
0.0620067121426169,0.0630819969569995,0.0730857845910175,0.0834236143414073,
0.093761444091797,0.118957117023634,0.124997637865204),.UNSPECIFIED.);
#1079=B_SPLINE_CURVE_WITH_KNOTS('',3,(#25838,#25839,#25840,#25841,#25842,
#25843,#25844,#25845,#25846,#25847,#25848,#25849,#25850,#25851,#25852,#25853,
#25854,#25855,#25856,#25857,#25858,#25859,#25860,#25861,#25862,#25863,#25864,
#25865,#25866,#25867,#25868,#25869,#25870,#25871,#25872,#25873,#25874,#25875,
#25876,#25877,#25878,#25879,#25880,#25881,#25882,#25883,#25884,#25885,#25886,
#25887,#25888,#25889),.UNSPECIFIED.,.F.,.F.,(4,3,3,3,3,3,3,3,3,3,3,3,3,
3,3,3,3,4),(0.875010334230379,0.875015258789063,0.885063223983587,0.895662334037692,
0.906261444091797,0.915329176293059,0.924362963681523,0.933304455697802,
0.935941078938443,0.937102710968539,0.938038619544317,0.948083027116603,
0.95824477230157,0.968683579226177,0.978878572825813,0.989439286412907,
0.999400899492149,1.),.UNSPECIFIED.);
#1080=B_SPLINE_CURVE_WITH_KNOTS('',3,(#25891,#25892,#25893,#25894,#25895,
#25896,#25897,#25898,#25899,#25900,#25901,#25902,#25903,#25904,#25905,#25906,
#25907,#25908,#25909,#25910,#25911,#25912,#25913,#25914,#25915,#25916,#25917,
#25918,#25919,#25920,#25921,#25922,#25923,#25924,#25925,#25926,#25927,#25928,
#25929,#25930,#25931,#25932,#25933,#25934,#25935,#25936,#25937,#25938,#25939,
#25940,#25941,#25942),.UNSPECIFIED.,.F.,.F.,(4,3,3,3,3,3,3,3,3,3,3,3,3,
3,3,3,3,4),(0.750027510254452,0.750030180562894,0.750030517578125,0.760114469760994,
0.770326204646331,0.780875375530647,0.791169951965582,0.801846420074588,
0.811924599407989,0.812522888183594,0.822590381964961,0.832779920362826,
0.84333280346223,0.853563394247635,0.863720399981247,0.873715992551155,
0.874991452760439,0.875010334230379),.UNSPECIFIED.);
#1081=B_SPLINE_CURVE_WITH_KNOTS('',3,(#25944,#25945,#25946,#25947,#25948,
#25949,#25950,#25951,#25952,#25953,#25954,#25955,#25956,#25957,#25958,#25959,
#25960,#25961,#25962,#25963,#25964,#25965,#25966,#25967,#25968,#25969,#25970,
#25971,#25972,#25973,#25974,#25975,#25976,#25977,#25978,#25979,#25980,#25981,
#25982,#25983,#25984,#25985,#25986,#25987,#25988,#25989),.UNSPECIFIED.,
 .F.,.F.,(4,3,3,3,3,3,3,3,3,3,3,3,3,3,3,4),(0.625035680662314,0.625045776367188,
0.634959360244037,0.645005190259783,0.655638429438002,0.66577810723537,
0.675860402489048,0.685791959316116,0.687538146972657,0.697444002791749,
0.707465979715092,0.71754735415445,0.727602770201362,0.737586421487148,
0.747408036910529,0.750027510254452),.UNSPECIFIED.);
#1082=B_SPLINE_CURVE_WITH_KNOTS('',3,(#25991,#25992,#25993,#25994,#25995,
#25996,#25997,#25998,#25999,#26000,#26001,#26002,#26003,#26004,#26005,#26006,
#26007,#26008,#26009,#26010,#26011,#26012,#26013,#26014,#26015,#26016,#26017,
#26018,#26019,#26020,#26021,#26022,#26023,#26024,#26025,#26026,#26027,#26028,
#26029,#26030,#26031,#26032,#26033,#26034,#26035,#26036,#26037,#26038,#26039,
#26040,#26041,#26042,#26043,#26044,#26045),.UNSPECIFIED.,.F.,.F.,(4,3,3,
3,3,3,3,3,3,3,3,3,3,3,3,3,3,3,4),(0.500061035156251,0.509784082219549,0.519668083969381,
0.529684204027609,0.539699455781287,0.549643684996335,0.559453770503833,
0.561600384288871,0.562427817012746,0.563166095090099,0.572935702006583,
0.582817729960924,0.592779134388661,0.593799591064454,0.602508339696414,
0.611153433496651,0.619637704379647,0.625016883677845,0.625035680662314),
 .UNSPECIFIED.);
#1083=B_SPLINE_CURVE_WITH_KNOTS('',3,(#26047,#26048,#26049,#26050,#26051,
#26052,#26053,#26054,#26055,#26056,#26057,#26058,#26059,#26060,#26061,#26062,
#26063,#26064,#26065,#26066,#26067,#26068,#26069,#26070,#26071,#26072,#26073,
#26074,#26075,#26076,#26077,#26078,#26079,#26080,#26081,#26082,#26083,#26084,
#26085,#26086,#26087,#26088,#26089,#26090,#26091,#26092),.UNSPECIFIED.,
 .F.,.F.,(4,3,3,3,3,3,3,3,3,3,3,3,3,3,3,4),(0.375039662445796,0.375045776367188,
0.385157469228026,0.395395289459459,0.405934818535024,0.416252083475239,
0.426902744618479,0.437004013717147,0.437553405761719,0.447532078985895,
0.45761507319284,0.4677726888567,0.468807220458985,0.491821180845468,0.500004452744443,
0.500032744006821),.UNSPECIFIED.);
#1084=B_SPLINE_CURVE_WITH_KNOTS('',3,(#26094,#26095,#26096,#26097,#26098,
#26099,#26100,#26101,#26102,#26103,#26104,#26105,#26106,#26107,#26108,#26109,
#26110,#26111,#26112,#26113,#26114,#26115,#26116,#26117,#26118,#26119,#26120,
#26121,#26122,#26123,#26124,#26125,#26126,#26127,#26128,#26129,#26130,#26131,
#26132,#26133,#26134,#26135,#26136,#26137,#26138,#26139),.UNSPECIFIED.,
 .F.,.F.,(4,3,3,3,3,3,3,3,3,3,3,3,3,3,3,4),(0.250040203921046,0.260006897061865,
0.270104787324373,0.280713127236444,0.290902669953587,0.301034854339568,
0.311017727734801,0.312538146972657,0.322520836674231,0.332620319240001,
0.34322347142839,0.353356467748657,0.363416849810154,0.373318487372145,
0.375032927993557,0.375039662445796),.UNSPECIFIED.);
#1085=B_SPLINE_CURVE_WITH_KNOTS('',3,(#26158,#26159,#26160,#26161,#26162,
#26163,#26164,#26165),.UNSPECIFIED.,.F.,.F.,(4,2,2,4),(1.88326006932265,
1.88351436623439,2.07186580148184,2.2601469129838),.UNSPECIFIED.);
#1086=B_SPLINE_CURVE_WITH_KNOTS('',3,(#26167,#26168,#26169,#26170,#26171,
#26172,#26173,#26174),.UNSPECIFIED.,.F.,.F.,(4,2,2,4),(1.50654556057706,
1.50681149115286,1.69516292869362,1.88326006932265),.UNSPECIFIED.);
#1087=B_SPLINE_CURVE_WITH_KNOTS('',3,(#26176,#26177,#26178,#26179,#26180,
#26181),.UNSPECIFIED.,.F.,.F.,(4,2,4),(1.13015385044563,1.31846005361209,
1.50654556057706),.UNSPECIFIED.);
#1088=B_SPLINE_CURVE_WITH_KNOTS('',3,(#26183,#26184,#26185,#26186,#26187,
#26188),.UNSPECIFIED.,.F.,.F.,(4,2,4),(0.753405745576428,0.941757180823877,
1.13010861607133),.UNSPECIFIED.);
#1089=B_SPLINE_CURVE_WITH_KNOTS('',3,(#26190,#26191,#26192,#26193,#26194,
#26195,#26196,#26197),.UNSPECIFIED.,.F.,.F.,(4,2,2,4),(0.376303807212213,
0.376702875081531,0.565054310328979,0.753405745576428),.UNSPECIFIED.);
#1090=B_SPLINE_CURVE_WITH_KNOTS('',3,(#26199,#26200,#26201,#26202,#26203,
#26204,#26205,#26206,#26207),.UNSPECIFIED.,.F.,.F.,(4,3,2,4),(3.01311448574183,
3.01362298230571,3.20197441984648,3.38992678951793),.UNSPECIFIED.);
#1091=B_SPLINE_CURVE_WITH_KNOTS('',3,(#26209,#26210,#26211,#26212,#26213,
#26214,#26215,#26216),.UNSPECIFIED.,.F.,.F.,(4,2,2,4),(2.63643507955563,
2.63692010722418,2.82527154476495,3.01311448574183),.UNSPECIFIED.);
#1092=B_SPLINE_CURVE_WITH_KNOTS('',3,(#26217,#26218,#26219,#26220,#26221,
#26222),.UNSPECIFIED.,.F.,.F.,(4,2,4),(2.26021723672928,2.44856867197673,
2.63643507955563),.UNSPECIFIED.);
#1093=B_SPLINE_CURVE_WITH_KNOTS('',3,(#26256,#26257,#26258,#26259),
 .UNSPECIFIED.,.F.,.F.,(4,4),(0.874999999999996,1.),.UNSPECIFIED.);
#1094=B_SPLINE_CURVE_WITH_KNOTS('',3,(#26261,#26262,#26263,#26264),
 .UNSPECIFIED.,.F.,.F.,(4,4),(0.,0.124999999999996),.UNSPECIFIED.);
#1095=B_SPLINE_CURVE_WITH_KNOTS('',3,(#26266,#26267,#26268,#26269),
 .UNSPECIFIED.,.F.,.F.,(4,4),(0.124999999999996,0.249999999999992),
 .UNSPECIFIED.);
#1096=B_SPLINE_CURVE_WITH_KNOTS('',3,(#26271,#26272,#26273,#26274),
 .UNSPECIFIED.,.F.,.F.,(4,4),(0.249999999999992,0.374999999999988),
 .UNSPECIFIED.);
#1097=B_SPLINE_CURVE_WITH_KNOTS('',3,(#26276,#26277,#26278,#26279,#26280,
#26281),.UNSPECIFIED.,.F.,.F.,(4,2,4),(0.375000000250893,0.499999999999984,
0.500028277877377),.UNSPECIFIED.);
#1098=B_SPLINE_CURVE_WITH_KNOTS('',3,(#26283,#26284,#26285,#26286),
 .UNSPECIFIED.,.F.,.F.,(4,4),(0.50005655573509,0.624999999999988),
 .UNSPECIFIED.);
#1099=B_SPLINE_CURVE_WITH_KNOTS('',3,(#26288,#26289,#26290,#26291),
 .UNSPECIFIED.,.F.,.F.,(4,4),(0.624999999999988,0.749999999999992),
 .UNSPECIFIED.);
#1100=B_SPLINE_CURVE_WITH_KNOTS('',3,(#26293,#26294,#26295,#26296),
 .UNSPECIFIED.,.F.,.F.,(4,4),(0.749999999999992,0.874999999999996),
 .UNSPECIFIED.);
#1101=B_SPLINE_CURVE_WITH_KNOTS('',3,(#26320,#26321,#26322,#26323,#26324,
#26325,#26326,#26327,#26328,#26329,#26330,#26331,#26332,#26333,#26334,#26335,
#26336,#26337,#26338,#26339,#26340,#26341,#26342,#26343),.UNSPECIFIED.,
 .F.,.F.,(4,2,2,2,2,2,2,2,2,2,2,4),(0.,0.103381366704768,0.206922202201336,
0.391377450354442,0.488690558489562,0.58707753918209,0.772543406462477,
0.970634500277933,1.19532551051909,1.24886321535489,1.45372318457095,1.6598018219901),
 .UNSPECIFIED.);
#1102=B_SPLINE_CURVE_WITH_KNOTS('',3,(#26390,#26391,#26392,#26393,#26394,
#26395,#26396,#26397,#26398,#26399,#26400,#26401,#26402,#26403,#26404,#26405,
#26406,#26407,#26408,#26409,#26410,#26411,#26412,#26413,#26414,#26415,#26416,
#26417,#26418,#26419,#26420,#26421,#26422,#26423,#26424,#26425,#26426,#26427,
#26428,#26429,#26430,#26431,#26432,#26433,#26434,#26435,#26436,#26437,#26438,
#26439,#26440,#26441,#26442,#26443,#26444,#26445,#26446,#26447,#26448,#26449,
#26450,#26451,#26452,#26453,#26454,#26455,#26456,#26457,#26458,#26459,#26460,
#26461,#26462,#26463,#26464,#26465,#26466,#26467,#26468,#26469,#26470,#26471,
#26472,#26473,#26474,#26475,#26476,#26477,#26478,#26479,#26480,#26481,#26482,
#26483,#26484,#26485,#26486,#26487,#26488,#26489,#26490,#26491,#26492,#26493,
#26494,#26495,#26496,#26497,#26498,#26499,#26500,#26501,#26502,#26503,#26504,
#26505,#26506,#26507,#26508,#26509,#26510,#26511,#26512,#26513,#26514,#26515,
#26516,#26517,#26518,#26519,#26520,#26521,#26522,#26523,#26524,#26525,#26526,
#26527,#26528,#26529,#26530,#26531,#26532,#26533,#26534,#26535,#26536,#26537,
#26538,#26539,#26540,#26541,#26542,#26543,#26544,#26545,#26546,#26547,#26548,
#26549,#26550,#26551,#26552,#26553,#26554,#26555,#26556,#26557,#26558,#26559,
#26560,#26561),.UNSPECIFIED.,.F.,.F.,(4,3,3,3,3,3,3,3,3,3,3,3,3,3,3,3,3,
3,3,3,3,3,3,3,3,3,3,3,3,3,3,3,3,3,3,3,3,3,3,3,3,3,3,3,3,3,3,3,3,3,3,3,3,
3,3,3,3,4),(0.,0.000315375744567924,0.000645903817980758,0.000976431891393592,
0.0012812537484511,0.00158740068641533,0.00189480456358316,0.00195286378278718,
0.00227229401054678,0.00260079484236378,0.00292929567418078,0.00320274758832941,
0.00347469402173951,0.00374433547800945,0.00390572756557437,0.00390584133492772,
0.00421689206020479,0.00453088806273884,0.00484662827091633,0.00488215945696796,
0.00525366301006075,0.00562563969088054,0.00585859134836155,0.00638053264119389,
0.00683502323975515,0.00715062223032276,0.00748103868073575,0.00779159828439098,
0.00781145513114874,0.00781203150209657,0.00808972377000141,0.00836905928236821,
0.00865075449187036,0.00878788702254233,0.00910517886612052,0.00943474889002822,
0.00976431891393592,0.0100622297668594,0.0103592836570688,0.0106546119602171,
0.0107407508053295,0.0110626953843491,0.0113899390405361,0.0117171826967231,
0.0117180975894192,0.0121313722590175,0.0125539529147115,0.0126936145881167,
0.0130183666566513,0.0133457392744377,0.0136700464795103,0.0139888224703152,
0.0143176504206095,0.0146464783709039,0.014919070754581,0.015190101683422,
0.0154587424133886,0.0156229102622975),.UNSPECIFIED.);
#1103=B_SPLINE_CURVE_WITH_KNOTS('',3,(#26602,#26603,#26604,#26605),
 .UNSPECIFIED.,.F.,.F.,(4,4),(-0.00017716250113245,0.),.UNSPECIFIED.);
#1104=B_SPLINE_CURVE_WITH_KNOTS('',3,(#26609,#26610,#26611,#26612,#26613,
#26614,#26615,#26616,#26617,#26618,#26619,#26620,#26621,#26622,#26623,#26624,
#26625,#26626,#26627,#26628,#26629,#26630,#26631,#26632),.UNSPECIFIED.,
 .F.,.F.,(4,2,2,2,2,2,2,2,2,2,2,4),(-1.65980182253606,-1.45372318489466,
-1.24886321541509,-1.19532551060548,-0.970634500303615,-0.772543406460149,
-0.587077539177558,-0.488690558484114,-0.391377450348774,-0.20692220219487,
-0.103381366701537,-0.00017716250113245),.UNSPECIFIED.);
#1105=B_SPLINE_CURVE_WITH_KNOTS('',3,(#26633,#26634,#26635,#26636,#26637,
#26638,#26639,#26640,#26641,#26642,#26643,#26644,#26645,#26646,#26647,#26648,
#26649,#26650,#26651,#26652,#26653,#26654,#26655,#26656,#26657,#26658,#26659,
#26660,#26661,#26662,#26663,#26664,#26665,#26666,#26667,#26668,#26669,#26670,
#26671,#26672,#26673,#26674,#26675,#26676,#26677,#26678,#26679,#26680,#26681,
#26682,#26683,#26684,#26685,#26686,#26687,#26688,#26689,#26690,#26691,#26692,
#26693,#26694,#26695,#26696,#26697,#26698,#26699,#26700,#26701,#26702,#26703,
#26704,#26705,#26706,#26707,#26708,#26709,#26710,#26711,#26712,#26713,#26714,
#26715,#26716,#26717,#26718,#26719,#26720,#26721,#26722,#26723,#26724,#26725,
#26726,#26727,#26728,#26729,#26730,#26731,#26732,#26733,#26734,#26735,#26736,
#26737,#26738,#26739,#26740,#26741,#26742,#26743,#26744,#26745,#26746,#26747,
#26748,#26749,#26750,#26751,#26752,#26753,#26754,#26755,#26756,#26757,#26758,
#26759,#26760,#26761,#26762,#26763,#26764,#26765,#26766,#26767,#26768,#26769,
#26770,#26771,#26772,#26773,#26774,#26775,#26776,#26777,#26778,#26779,#26780,
#26781,#26782,#26783,#26784,#26785,#26786,#26787,#26788,#26789,#26790,#26791,
#26792,#26793,#26794,#26795,#26796,#26797,#26798,#26799,#26800,#26801,#26802,
#26803,#26804),.UNSPECIFIED.,.F.,.F.,(4,3,3,3,3,3,3,3,3,3,3,3,3,3,3,3,3,
3,3,3,3,3,3,3,3,3,3,3,3,3,3,3,3,3,3,3,3,3,3,3,3,3,3,3,3,3,3,3,3,3,3,3,3,
3,3,3,3,4),(4.21060351010033E-19,0.000315375742575029,0.000645903817003116,
0.000976431891431204,0.00128125374781883,0.00158740068510089,0.0018948045615801,
0.00195286378286241,0.00227229401064095,0.00260079484246728,0.00292929567429361,
0.00320274758882887,0.00347469402262506,0.00374433547927827,0.00390572756572481,
0.00390584133502637,0.00421689206038293,0.00453088806297221,0.00484662827116357,
0.00488215945715601,0.00525366301724405,0.00562563970480409,0.00585859134858722,
0.00638053260631128,0.00683502324001842,0.00715062223061402,0.00748103868103182,
0.0077915982846478,0.00781145513144962,0.00781203150237952,0.00808972376946302,
0.00836905928099522,0.00865075448965919,0.00878788702288083,0.00910517886651736,
0.0094347488904147,0.00976431891431203,0.0100622297685835,0.01035928366013,
0.0106546119645884,0.0107407508057432,0.0110626953846664,0.0113899390409204,
0.0117171826971744,0.0117180975897762,0.01213137223928,0.0125539528739886,
0.0126936145886056,0.0130183666541618,0.0133457392688836,0.0136700464800368,
0.0139888224708903,0.0143176504211792,0.014646478371468,0.0149190707552556,
0.015190101684208,0.0154587424142883,0.0156229102628992),.UNSPECIFIED.);
#1106=B_SPLINE_CURVE_WITH_KNOTS('',3,(#27167,#27168,#27169,#27170,#27171,
#27172,#27173,#27174,#27175,#27176,#27177,#27178,#27179,#27180,#27181,#27182,
#27183,#27184,#27185,#27186,#27187,#27188,#27189,#27190,#27191,#27192,#27193,
#27194,#27195,#27196,#27197,#27198,#27199,#27200,#27201,#27202,#27203,#27204,
#27205,#27206,#27207,#27208,#27209,#27210,#27211,#27212,#27213,#27214,#27215,
#27216,#27217,#27218,#27219,#27220,#27221,#27222,#27223,#27224,#27225,#27226,
#27227,#27228,#27229,#27230,#27231,#27232,#27233,#27234,#27235,#27236,#27237,
#27238,#27239,#27240,#27241,#27242,#27243,#27244,#27245,#27246,#27247,#27248,
#27249,#27250,#27251,#27252,#27253,#27254,#27255,#27256,#27257,#27258,#27259,
#27260,#27261,#27262,#27263,#27264,#27265,#27266),.UNSPECIFIED.,.F.,.F.,
(4,3,3,3,3,3,3,3,3,3,3,3,3,3,3,3,3,3,3,3,3,3,3,3,3,3,3,3,3,3,3,3,3,4),(0.460209507152456,
0.461151420671335,0.462093334190213,0.462902601160825,0.462955010568935,
0.463641386423054,0.464002099657692,0.464327762277174,0.464886176252622,
0.465429272087291,0.465700513985413,0.465946575674178,0.466383479195188,
0.466806080207127,0.466953830111869,0.467073265693652,0.467448107915379,
0.467815545281024,0.467998655841874,0.468322253700499,0.468446017401892,
0.468744114624328,0.469031905032931,0.469096950144427,0.469132393256011,
0.469479983587368,0.469671620413561,0.469818769110131,0.470094277283303,
0.470264386451509,0.470633430176549,0.4708701753027,0.471160215519294,0.47119152081837),
 .UNSPECIFIED.);
#1107=B_SPLINE_CURVE_WITH_KNOTS('',3,(#27268,#27269,#27270,#27271,#27272,
#27273,#27274,#27275,#27276,#27277,#27278,#27279,#27280,#27281,#27282,#27283,
#27284,#27285,#27286,#27287,#27288,#27289,#27290,#27291,#27292,#27293,#27294,
#27295,#27296,#27297,#27298,#27299,#27300,#27301,#27302,#27303,#27304,#27305,
#27306,#27307,#27308,#27309,#27310,#27311,#27312,#27313,#27314,#27315,#27316,
#27317,#27318,#27319,#27320,#27321,#27322,#27323,#27324,#27325,#27326,#27327,
#27328,#27329,#27330,#27331,#27332,#27333,#27334,#27335,#27336,#27337,#27338,
#27339,#27340,#27341,#27342,#27343,#27344,#27345),.UNSPECIFIED.,.F.,.F.,
(4,2,2,2,2,2,2,2,2,2,2,2,2,2,2,2,2,2,2,2,2,2,2,2,2,2,2,2,2,2,2,2,2,2,2,
2,2,2,4),(0.238679919152522,0.239545269105647,0.240410619058772,0.241275969011897,
0.242141318965021,0.243872018871271,0.24560271877752,0.24733341868377,0.249064118590019,
0.252525518402518,0.255986918215017,0.259448318027516,0.266371117652514,
0.269832517465013,0.273293917277512,0.28021671690251,0.294062316152505,
0.307907915402501,0.314830715027499,0.318292114839998,0.321753514652497,
0.335599113902493,0.349444713152489,0.363290312402485,0.366751712214984,
0.370213112027483,0.377135911652481,0.390981510902477,0.404827110152473,
0.418672709402469,0.422134109214968,0.425595509027467,0.432518308652464,
0.439441108277462,0.44636390790246,0.449825307714959,0.453286707527458,
0.456748107339957,0.460209507152456),.UNSPECIFIED.);
#1108=B_SPLINE_CURVE_WITH_KNOTS('',3,(#27352,#27353,#27354,#27355,#27356,
#27357,#27358,#27359,#27360,#27361,#27362,#27363,#27364,#27365,#27366,#27367),
 .UNSPECIFIED.,.F.,.F.,(4,2,2,2,2,2,2,4),(0.227148662184115,0.230031476426217,
0.232914290668319,0.23435569778937,0.235797104910421,0.237238512031472,
0.237959215591997,0.238679919152522),.UNSPECIFIED.);
#1109=B_SPLINE_CURVE_WITH_KNOTS('',3,(#27368,#27369,#27370,#27371,#27372,
#27373,#27374,#27375,#27376,#27377,#27378,#27379,#27380,#27381,#27382,#27383,
#27384,#27385,#27386,#27387,#27388,#27389,#27390,#27391,#27392,#27393,#27394,
#27395,#27396,#27397,#27398,#27399,#27400,#27401,#27402,#27403,#27404,#27405,
#27406,#27407,#27408,#27409,#27410,#27411,#27412,#27413,#27414,#27415,#27416,
#27417,#27418,#27419,#27420,#27421,#27422,#27423,#27424,#27425,#27426,#27427,
#27428,#27429,#27430,#27431,#27432,#27433,#27434,#27435,#27436,#27437,#27438,
#27439,#27440,#27441,#27442,#27443,#27444,#27445),.UNSPECIFIED.,.F.,.F.,
(4,2,2,2,2,2,2,2,2,2,2,2,2,2,2,2,2,2,2,2,2,2,2,2,2,2,2,2,2,2,2,2,2,2,2,
2,2,2,4),(0.00739566262098398,0.00825407277552746,0.00911248293007093,0.00997089308461441,
0.0108293032391579,0.0116877133937014,0.0125461235482448,0.0142629438573318,
0.0176965844755058,0.0194134047845928,0.0211302250936798,0.0245638657118537,
0.0279975063300277,0.0348647875663756,0.0382984281845495,0.0417320688027234,
0.0485993500390712,0.0623339125117668,0.0760684749844625,0.0829357562208103,
0.0863693968389842,0.0898030374571581,0.103537599929854,0.117272162402549,
0.131006724875245,0.137874006111593,0.144741287347941,0.158475849820636,
0.172210412293332,0.185944974766028,0.189378615384202,0.192812256002376,
0.199679537238724,0.206546818475071,0.213414099711419,0.216847740329593,
0.220281380947767,0.223715021565941,0.227148662184115),.UNSPECIFIED.);
#1110=B_SPLINE_CURVE_WITH_KNOTS('',3,(#27455,#27456,#27457,#27458,#27459,
#27460,#27461,#27462,#27463,#27464,#27465,#27466,#27467,#27468,#27469,#27470,
#27471,#27472,#27473,#27474,#27475,#27476,#27477,#27478,#27479,#27480,#27481,
#27482,#27483,#27484,#27485,#27486,#27487,#27488,#27489,#27490,#27491,#27492,
#27493,#27494,#27495,#27496,#27497,#27498,#27499,#27500,#27501,#27502,#27503,
#27504,#27505,#27506,#27507,#27508,#27509,#27510,#27511,#27512,#27513,#27514,
#27515,#27516,#27517,#27518,#27519,#27520,#27521,#27522,#27523,#27524,#27525,
#27526,#27527,#27528,#27529,#27530),.UNSPECIFIED.,.F.,.F.,(4,2,2,2,2,2,
2,2,2,2,2,2,2,2,2,2,2,2,2,2,2,2,2,2,2,2,2,2,2,2,2,2,2,2,2,2,2,4),(0.00794038585254472,
0.00880514189733557,0.00966989794212641,0.0105346539869173,0.0113994100317081,
0.0122641660764989,0.0131289221212898,0.0148584342108715,0.0183174583900349,
0.0217764825691984,0.0252355067483618,0.0286945309275253,0.0356125792858521,
0.0390716034650155,0.0425306276441789,0.0494486760025058,0.0632847727191596,
0.0771208694358133,0.0840389177941402,0.0909569661524671,0.104793062869121,
0.118629159585775,0.132465256302429,0.135924280481592,0.139383304660755,
0.146301353019082,0.160137449735736,0.17397354645239,0.187809643169044,
0.191268667348207,0.19472769152737,0.201645739885697,0.208563788244024,
0.215481836602351,0.218940860781514,0.222399884960678,0.225858909139841,
0.229317933319005),.UNSPECIFIED.);
#1111=B_SPLINE_CURVE_WITH_KNOTS('',3,(#27532,#27533,#27534,#27535,#27536,
#27537,#27538,#27539,#27540,#27541,#27542,#27543,#27544,#27545,#27546,#27547,
#27548,#27549,#27550,#27551,#27552,#27553,#27554,#27555,#27556,#27557,#27558,
#27559,#27560,#27561,#27562,#27563,#27564,#27565,#27566,#27567,#27568,#27569,
#27570,#27571,#27572,#27573,#27574,#27575,#27576,#27577,#27578,#27579,#27580,
#27581,#27582,#27583,#27584,#27585,#27586,#27587,#27588,#27589,#27590,#27591,
#27592,#27593,#27594,#27595,#27596,#27597,#27598,#27599,#27600,#27601,#27602,
#27603,#27604,#27605,#27606,#27607,#27608,#27609,#27610,#27611,#27612,#27613,
#27614,#27615,#27616,#27617,#27618,#27619,#27620,#27621,#27622,#27623,#27624,
#27625,#27626,#27627,#27628),.UNSPECIFIED.,.F.,.F.,(4,3,3,3,3,3,3,3,3,3,
3,3,3,3,3,3,3,3,3,3,3,3,3,3,3,3,3,3,3,3,3,3,4),(0.229317933319005,0.230219578872938,
0.231090137167458,0.2312226752802,0.231993548591037,0.232168511536746,0.232709951257979,
0.233162059154581,0.233593800645616,0.234128304964287,0.23464985746595,
0.235019089754487,0.235170367762224,0.235605699057557,0.236029101015188,
0.236218790613006,0.236444378863357,0.236828028579282,0.237209220341014,
0.237314371101707,0.237650300518339,0.237869667972228,0.238217872028818,
0.238476872425152,0.238822259812058,0.239089125159825,0.239294957081098,
0.239577620782566,0.239723674920968,0.240110911517401,0.240374392336933,
0.240670477938072,0.240720246189969),.UNSPECIFIED.);
#1112=B_SPLINE_CURVE_WITH_KNOTS('',3,(#27635,#27636,#27637,#27638,#27639,
#27640,#27641,#27642,#27643,#27644,#27645,#27646,#27647,#27648,#27649,#27650,
#27651,#27652,#27653,#27654,#27655,#27656,#27657,#27658,#27659,#27660,#27661,
#27662,#27663,#27664,#27665,#27666,#27667,#27668,#27669,#27670,#27671,#27672,
#27673,#27674,#27675,#27676,#27677,#27678,#27679,#27680,#27681,#27682,#27683,
#27684,#27685,#27686,#27687,#27688,#27689,#27690,#27691,#27692,#27693,#27694,
#27695,#27696,#27697,#27698,#27699,#27700,#27701,#27702,#27703,#27704,#27705,
#27706,#27707,#27708,#27709,#27710),.UNSPECIFIED.,.F.,.F.,(4,2,2,2,2,2,
2,2,2,2,2,2,2,2,2,2,2,2,2,2,2,2,2,2,2,2,2,2,2,2,2,2,2,2,2,2,2,4),(0.240720246189969,
0.241587257099786,0.242454268009604,0.244188289829239,0.245055300739056,
0.245922311648874,0.247656333468509,0.251124377107779,0.252858398927414,
0.254592420747049,0.258060464386319,0.261528508025589,0.268464595304129,
0.271932638943399,0.275400682582669,0.282336769861209,0.29620894441829,
0.31008111897537,0.31701720625391,0.32048524989318,0.32395329353245,0.33782546808953,
0.351697642646611,0.365569817203691,0.372505904482231,0.379441991760771,
0.393314166317851,0.407186340874931,0.421058515432011,0.424526559071281,
0.427994602710552,0.434930689989092,0.441866777267632,0.448802864546172,
0.452270908185442,0.455738951824712,0.459206995463982,0.462675039103252),
 .UNSPECIFIED.);
#1113=B_SPLINE_CURVE_WITH_KNOTS('',3,(#27711,#27712,#27713,#27714,#27715,
#27716,#27717,#27718,#27719,#27720,#27721,#27722,#27723,#27724,#27725,#27726,
#27727,#27728,#27729,#27730,#27731,#27732,#27733,#27734,#27735,#27736,#27737,
#27738,#27739,#27740,#27741,#27742,#27743,#27744,#27745,#27746,#27747,#27748,
#27749,#27750,#27751,#27752,#27753,#27754,#27755,#27756,#27757,#27758,#27759,
#27760,#27761,#27762,#27763,#27764,#27765,#27766,#27767,#27768,#27769,#27770,
#27771,#27772,#27773,#27774,#27775,#27776,#27777,#27778,#27779,#27780,#27781,
#27782,#27783,#27784,#27785,#27786,#27787,#27788,#27789,#27790,#27791,#27792,
#27793,#27794,#27795,#27796,#27797,#27798,#27799,#27800,#27801,#27802,#27803,
#27804,#27805,#27806,#27807,#27808,#27809,#27810,#27811,#27812,#27813),
 .UNSPECIFIED.,.F.,.F.,(4,3,3,3,3,3,3,3,3,3,3,3,3,3,3,3,3,3,3,3,3,3,3,3,
3,3,3,3,3,3,3,3,3,3,4),(0.462675039103252,0.463642750480073,0.46457571174879,
0.465419810646746,0.465637485084959,0.466378096580386,0.46650737588057,
0.466828801914374,0.467118708075813,0.467646311136065,0.46816291669427,
0.468463738208056,0.468599931066666,0.469042894113483,0.4694858571603,0.469885588555766,
0.47008115405752,0.470495888471532,0.470551832133678,0.470927952128342,
0.471304862088803,0.471562377048373,0.471673225717309,0.471998870547497,
0.472322619053715,0.472644470724174,0.472868538651809,0.473043600039227,
0.473311697268788,0.473502563110719,0.473784211534654,0.474111751611527,
0.474153415877385,0.474442628569102,0.474524823030081),.UNSPECIFIED.);
#1114=B_SPLINE_CURVE_WITH_KNOTS('',3,(#28104,#28105,#28106,#28107,#28108,
#28109,#28110,#28111,#28112,#28113,#28114,#28115,#28116,#28117,#28118,#28119,
#28120,#28121,#28122,#28123,#28124,#28125,#28126,#28127,#28128,#28129,#28130,
#28131,#28132,#28133,#28134,#28135,#28136,#28137,#28138,#28139,#28140,#28141,
#28142,#28143,#28144,#28145,#28146,#28147,#28148,#28149,#28150,#28151,#28152,
#28153,#28154,#28155,#28156,#28157,#28158,#28159,#28160,#28161,#28162,#28163,
#28164,#28165,#28166,#28167,#28168,#28169,#28170,#28171,#28172,#28173,#28174,
#28175,#28176,#28177,#28178,#28179,#28180,#28181,#28182,#28183,#28184,#28185,
#28186,#28187,#28188,#28189,#28190,#28191,#28192,#28193,#28194,#28195,#28196,
#28197,#28198,#28199,#28200,#28201,#28202,#28203,#28204,#28205,#28206,#28207,
#28208,#28209,#28210,#28211,#28212,#28213,#28214,#28215,#28216,#28217,#28218,
#28219,#28220,#28221,#28222,#28223,#28224,#28225,#28226,#28227,#28228,#28229,
#28230,#28231,#28232,#28233,#28234,#28235,#28236,#28237,#28238,#28239,#28240,
#28241,#28242,#28243,#28244,#28245,#28246,#28247,#28248,#28249,#28250,#28251,
#28252,#28253,#28254,#28255,#28256,#28257,#28258,#28259,#28260,#28261,#28262,
#28263,#28264,#28265,#28266,#28267,#28268,#28269,#28270,#28271,#28272,#28273,
#28274,#28275,#28276,#28277,#28278,#28279,#28280,#28281,#28282,#28283,#28284,
#28285,#28286,#28287,#28288,#28289,#28290,#28291,#28292,#28293,#28294,#28295,
#28296,#28297,#28298,#28299,#28300,#28301,#28302,#28303,#28304,#28305,#28306,
#28307,#28308,#28309,#28310,#28311,#28312,#28313,#28314,#28315,#28316,#28317,
#28318,#28319,#28320,#28321,#28322,#28323,#28324,#28325,#28326,#28327,#28328,
#28329,#28330,#28331,#28332,#28333,#28334,#28335,#28336,#28337,#28338,#28339,
#28340,#28341,#28342,#28343,#28344,#28345,#28346,#28347,#28348,#28349,#28350,
#28351,#28352,#28353,#28354,#28355,#28356,#28357,#28358,#28359,#28360,#28361,
#28362,#28363,#28364,#28365,#28366,#28367,#28368,#28369,#28370,#28371,#28372,
#28373,#28374),.UNSPECIFIED.,.F.,.F.,(4,3,3,3,3,3,3,3,3,3,3,3,3,3,3,3,3,
3,3,3,3,3,3,3,3,3,3,3,3,3,3,3,3,3,3,3,3,3,3,3,3,3,3,3,3,3,3,3,3,3,3,3,3,
3,3,3,3,3,3,3,3,3,3,3,3,3,3,3,3,3,3,3,3,3,3,3,3,3,3,3,3,3,3,3,3,3,3,3,3,
3,4),(0.224444858500095,0.22692744060886,0.227879496390915,0.230926240713455,
0.231314134281736,0.235244024646494,0.238183410063376,0.244065722262328,
0.245052685845016,0.250738517111399,0.251921961626656,0.256859015714205,
0.258791237408296,0.261072409990444,0.26336646159019,0.265660513189936,
0.269986768381055,0.2743274185893,0.278683851522941,0.279399064753217,0.283831667173853,
0.288484641745175,0.293137616316497,0.297522480509796,0.301898066219627,
0.306256408549942,0.306876167879778,0.312710660889063,0.313745443661418,
0.318006273157165,0.320614719443058,0.324985848032814,0.329367820397019,
0.333760180874338,0.334353271006338,0.338776399740954,0.343198036678773,
0.347612751200278,0.348091822569619,0.352412228570066,0.356719848561029,
0.361005562897052,0.361830374132899,0.365456509513952,0.36869964991454,
0.37311710254083,0.37556892569618,0.380066366428911,0.384686921844185,0.38930747725946,
0.393839857281756,0.398442943052248,0.403046028822741,0.404952521931736,
0.406480666713561,0.409915304604381,0.413625500232383,0.416784580386021,
0.419769424576158,0.420219218276841,0.422728197517123,0.423653856167661,
0.425371175113071,0.426528854434269,0.427088494058482,0.428483134892337,
0.428805813003892,0.429979788180236,0.430523131949302,0.431264106069434,
0.432038976771861,0.432240450894712,0.433018232487655,0.433099110367417,
0.433957769840122,0.434387099576474,0.434816429312827,0.435245759049179,
0.435675088785532,0.436104418521884,0.436533748258237,0.437164180274058,
0.437392407730942,0.438251067203647,0.43897915760757,0.439109726676352,
0.440209087477563,0.440827045621762,0.441983333957617,0.442544364567172,
0.444261683512582),.UNSPECIFIED.);
#1115=B_SPLINE_CURVE_WITH_KNOTS('',3,(#28693,#28694,#28695,#28696,#28697,
#28698,#28699,#28700,#28701,#28702,#28703,#28704,#28705,#28706,#28707,#28708,
#28709,#28710,#28711,#28712,#28713,#28714,#28715,#28716,#28717,#28718,#28719,
#28720,#28721,#28722,#28723,#28724,#28725,#28726,#28727,#28728,#28729,#28730,
#28731,#28732,#28733,#28734,#28735,#28736,#28737,#28738,#28739,#28740,#28741,
#28742,#28743,#28744,#28745,#28746,#28747,#28748,#28749,#28750,#28751,#28752,
#28753,#28754,#28755,#28756,#28757,#28758,#28759,#28760,#28761,#28762,#28763,
#28764,#28765,#28766,#28767,#28768,#28769,#28770,#28771,#28772,#28773,#28774,
#28775,#28776,#28777,#28778,#28779,#28780,#28781,#28782,#28783,#28784,#28785,
#28786,#28787,#28788,#28789,#28790,#28791,#28792,#28793,#28794,#28795,#28796,
#28797,#28798,#28799,#28800,#28801,#28802,#28803,#28804,#28805,#28806,#28807,
#28808,#28809,#28810,#28811,#28812,#28813,#28814,#28815,#28816,#28817,#28818,
#28819,#28820,#28821,#28822,#28823,#28824,#28825,#28826,#28827,#28828,#28829,
#28830,#28831,#28832,#28833,#28834,#28835,#28836,#28837,#28838,#28839,#28840,
#28841,#28842,#28843,#28844,#28845,#28846,#28847,#28848,#28849,#28850,#28851,
#28852,#28853,#28854,#28855,#28856,#28857,#28858,#28859,#28860,#28861,#28862,
#28863,#28864,#28865,#28866,#28867,#28868,#28869,#28870,#28871,#28872,#28873,
#28874,#28875,#28876,#28877,#28878,#28879,#28880,#28881,#28882,#28883,#28884,
#28885,#28886,#28887,#28888,#28889,#28890,#28891,#28892,#28893,#28894,#28895,
#28896,#28897,#28898,#28899,#28900,#28901,#28902,#28903,#28904,#28905,#28906,
#28907,#28908,#28909,#28910,#28911,#28912,#28913,#28914,#28915,#28916,#28917,
#28918,#28919,#28920,#28921,#28922,#28923,#28924,#28925,#28926,#28927,#28928,
#28929,#28930,#28931,#28932,#28933,#28934,#28935,#28936,#28937,#28938,#28939,
#28940,#28941,#28942,#28943,#28944,#28945,#28946,#28947,#28948,#28949,#28950,
#28951,#28952,#28953,#28954,#28955,#28956,#28957,#28958,#28959,#28960,#28961,
#28962,#28963,#28964,#28965,#28966,#28967,#28968,#28969,#28970,#28971,#28972,
#28973,#28974,#28975,#28976,#28977,#28978,#28979,#28980,#28981,#28982,#28983,
#28984,#28985,#28986,#28987,#28988,#28989,#28990,#28991,#28992,#28993,#28994,
#28995,#28996,#28997,#28998,#28999,#29000,#29001,#29002,#29003,#29004,#29005,
#29006,#29007,#29008,#29009,#29010,#29011,#29012,#29013,#29014,#29015,#29016,
#29017,#29018,#29019,#29020,#29021,#29022,#29023,#29024,#29025,#29026,#29027,
#29028,#29029,#29030,#29031,#29032,#29033,#29034,#29035,#29036,#29037,#29038,
#29039,#29040,#29041,#29042,#29043,#29044,#29045,#29046,#29047,#29048,#29049,
#29050,#29051,#29052,#29053,#29054,#29055,#29056,#29057,#29058,#29059,#29060,
#29061,#29062,#29063,#29064,#29065,#29066,#29067,#29068,#29069,#29070,#29071),
 .UNSPECIFIED.,.F.,.F.,(4,3,3,3,3,3,3,3,3,3,3,3,3,3,3,3,3,3,3,3,3,3,3,3,
3,3,3,3,3,3,3,3,3,3,3,3,3,3,3,3,3,3,3,3,3,3,3,3,3,3,3,3,3,3,3,3,3,3,3,3,
3,3,3,3,3,3,3,3,3,3,3,3,3,3,3,3,3,3,3,3,3,3,3,3,3,3,3,3,3,3,3,3,3,3,3,3,
3,3,3,3,3,3,3,3,3,3,3,3,3,3,3,3,3,3,3,3,3,3,3,3,3,3,3,3,3,3,4),(0.219197959928519,
0.221561939635842,0.222568084891394,0.222573536212963,0.225521953279716,
0.225938209854269,0.225945565409889,0.228899400741101,0.229308334817144,
0.229315162107022,0.232678459780019,0.232683807174909,0.23941870970577,
0.239419709772932,0.246154269068837,0.24615895963152,0.252887867831646,
0.25289920955727,0.256254394695028,0.256269334520146,0.259620875989218,
0.259639459483021,0.273086779141874,0.273119959334522,0.286552662168457,
0.286600459186022,0.300018539495296,0.300080959037523,0.303385007721931,
0.303451084000398,0.306751479243036,0.306821208963274,0.313484421786241,
0.313561458889024,0.326950319411585,0.327041958740525,0.340416230672734,
0.340522458592025,0.347149188045422,0.347262708517776,0.350515662378619,
0.350632833480651,0.353882144673237,0.354002958443526,0.367348212398027,
0.367483458295027,0.380814786959129,0.380963958146528,0.387548398940738,
0.394282341493094,0.394444457998029,0.397649472177266,0.397814582960904,
0.401016888220728,0.401184707923779,0.405374640221065,0.407754831391867,
0.40792495784953,0.410662353985238,0.411126004115685,0.411295082812405,
0.413791286746707,0.414499346528745,0.41466520777528,0.415976012040286,
0.416187126755619,0.416350270256718,0.41739616230529,0.417876132158158,
0.418035332738155,0.419036083859736,0.419567899304777,0.419720395219593,
0.420492219658592,0.421195376093865,0.421264044097592,0.42140545770103,
0.421878321078495,0.422114709919513,0.422247988941749,0.422778375402946,
0.422968274381381,0.423090520182468,0.423396677144126,0.423778766392894,
0.423826452478747,0.423933051423187,0.424179502894481,0.424257716513561,
0.424354317043546,0.424583239235609,0.424690806953789,0.424775582663906,
0.425008747616126,0.425124948394551,0.425196848284265,0.425433747395109,
0.425559819081613,0.425618113904624,0.425936254136417,0.425993896086829,
0.426039379524984,0.426322139644522,0.426426703567751,0.426460645145343,
0.426905273846551,0.427287123039787,0.427303176386062,0.427853616496466,
0.42814235868823,0.428145707626781,0.428662176887248,0.4289882388675,0.428993655368323,
0.429532687076055,0.429830770108219,0.429837872940089,0.430516322774704,
0.430673301348937,0.431009296324422,0.43137348857443,0.431509007896478,
0.431515832589656,0.432713569432477,0.433195104231628,0.434601834369309,
0.434885957552532),.UNSPECIFIED.);
#1116=B_SPLINE_CURVE_WITH_KNOTS('',3,(#29085,#29086,#29087,#29088,#29089,
#29090,#29091,#29092,#29093,#29094,#29095,#29096,#29097,#29098,#29099,#29100,
#29101,#29102,#29103,#29104,#29105,#29106,#29107,#29108,#29109,#29110,#29111,
#29112,#29113,#29114,#29115,#29116,#29117,#29118,#29119,#29120,#29121,#29122,
#29123,#29124,#29125,#29126,#29127,#29128,#29129,#29130,#29131,#29132,#29133,
#29134,#29135,#29136,#29137,#29138,#29139,#29140,#29141,#29142,#29143,#29144,
#29145,#29146,#29147,#29148,#29149,#29150,#29151,#29152,#29153,#29154,#29155,
#29156,#29157,#29158,#29159,#29160,#29161,#29162,#29163,#29164,#29165,#29166,
#29167,#29168,#29169,#29170,#29171,#29172,#29173,#29174,#29175,#29176,#29177,
#29178,#29179,#29180,#29181,#29182,#29183,#29184,#29185,#29186,#29187,#29188,
#29189,#29190,#29191,#29192,#29193,#29194,#29195,#29196,#29197,#29198,#29199,
#29200,#29201,#29202,#29203,#29204,#29205,#29206,#29207,#29208,#29209,#29210,
#29211,#29212,#29213,#29214,#29215,#29216,#29217,#29218,#29219,#29220,#29221,
#29222,#29223,#29224,#29225,#29226,#29227,#29228,#29229,#29230,#29231,#29232,
#29233,#29234,#29235,#29236,#29237,#29238,#29239,#29240,#29241,#29242,#29243,
#29244,#29245,#29246,#29247,#29248,#29249,#29250,#29251,#29252,#29253,#29254,
#29255,#29256,#29257,#29258,#29259,#29260,#29261,#29262,#29263,#29264,#29265,
#29266,#29267,#29268,#29269,#29270,#29271,#29272,#29273,#29274,#29275,#29276,
#29277,#29278,#29279,#29280,#29281,#29282,#29283,#29284,#29285,#29286,#29287,
#29288,#29289,#29290,#29291,#29292,#29293,#29294,#29295,#29296,#29297,#29298,
#29299,#29300,#29301,#29302,#29303,#29304,#29305,#29306,#29307,#29308,#29309,
#29310,#29311,#29312,#29313,#29314,#29315,#29316,#29317,#29318,#29319,#29320,
#29321,#29322,#29323,#29324,#29325,#29326,#29327,#29328,#29329,#29330,#29331,
#29332,#29333,#29334,#29335,#29336,#29337,#29338,#29339,#29340,#29341,#29342,
#29343,#29344,#29345,#29346,#29347,#29348,#29349,#29350,#29351,#29352,#29353,
#29354,#29355),.UNSPECIFIED.,.F.,.F.,(4,3,3,3,3,3,3,3,3,3,3,3,3,3,3,3,3,
3,3,3,3,3,3,3,3,3,3,3,3,3,3,3,3,3,3,3,3,3,3,3,3,3,3,3,3,3,3,3,3,3,3,3,3,
3,3,3,3,3,3,3,3,3,3,3,3,3,3,3,3,3,3,3,3,3,3,3,3,3,3,3,3,3,3,3,3,3,3,3,3,
3,4),(0.0034429235827854,0.00572320515136817,0.00681409602568749,0.00957936021906904,
0.0101852684685896,0.0136633472913732,0.0169276133543937,0.0216348837645216,
0.0236699582401979,0.0263702387236477,0.0290689423761318,0.0304123031260021,
0.0349964377927312,0.0371546480118062,0.0396086289033257,0.042063926447067,
0.0438969928976104,0.0481532478627733,0.0524236025363501,0.0567093502317182,
0.0573816826692188,0.06174126798354,0.0663038202121836,0.0708663724408272,
0.0751777428891207,0.0794798820405295,0.0837649362753547,0.0843510622124355,
0.0886023464618641,0.0910934070982397,0.0952853955230474,0.0978357519840439,
0.102135545828145,0.106445937902228,0.110766418873797,0.111320441755652,
0.115670199879133,0.120237665703197,0.124805131527261,0.129052845127648,
0.13328789796319,0.137501313256485,0.138289821298869,0.14219369664852,0.145032166184673,
0.149378357587458,0.151774511070477,0.156199296918911,0.160729248880498,
0.165259200842086,0.169719242146463,0.174231566380079,0.178743890613694,
0.180619504999544,0.182115063056596,0.185486235499498,0.189107659841198,
0.192228580385302,0.195144301436354,0.195599752828204,0.19805031374221,
0.198970925271106,0.200656511492557,0.201815686763459,0.202342097714009,
0.203704624246645,0.20402768393546,0.205173489201687,0.205713270156911,
0.206440715127883,0.207203427929388,0.207398856378362,0.208142330961523,
0.208241649489087,0.209084442599813,0.209505839155175,0.209927235710538,
0.210348632265901,0.210770028821264,0.211191425376626,0.211612821931989,
0.212239081157345,0.212455615042715,0.21329840815344,0.214011586971214,
0.214141201264166,0.215229565569696,0.215826787485617,0.216979396477024,
0.217512373707068,0.219197959928519),.UNSPECIFIED.);
#1117=B_SPLINE_CURVE_WITH_KNOTS('',3,(#29645,#29646,#29647,#29648,#29649,
#29650,#29651,#29652,#29653,#29654,#29655,#29656,#29657,#29658,#29659,#29660,
#29661,#29662,#29663,#29664,#29665,#29666,#29667,#29668,#29669,#29670,#29671,
#29672,#29673,#29674,#29675,#29676,#29677,#29678,#29679,#29680,#29681,#29682,
#29683,#29684,#29685,#29686,#29687,#29688,#29689,#29690,#29691,#29692,#29693,
#29694,#29695,#29696,#29697,#29698,#29699,#29700,#29701,#29702,#29703,#29704,
#29705,#29706,#29707,#29708,#29709,#29710,#29711,#29712,#29713,#29714,#29715,
#29716,#29717,#29718,#29719,#29720,#29721,#29722,#29723,#29724,#29725,#29726,
#29727,#29728,#29729,#29730,#29731,#29732,#29733,#29734,#29735,#29736,#29737,
#29738,#29739,#29740,#29741,#29742,#29743,#29744,#29745,#29746,#29747,#29748,
#29749,#29750,#29751,#29752,#29753,#29754,#29755,#29756,#29757,#29758,#29759,
#29760,#29761,#29762,#29763,#29764,#29765,#29766,#29767,#29768,#29769,#29770,
#29771,#29772,#29773,#29774,#29775,#29776,#29777,#29778,#29779,#29780,#29781,
#29782,#29783,#29784,#29785,#29786,#29787,#29788,#29789,#29790,#29791,#29792,
#29793,#29794,#29795,#29796,#29797,#29798,#29799,#29800,#29801,#29802,#29803,
#29804,#29805,#29806,#29807,#29808,#29809,#29810,#29811,#29812,#29813,#29814,
#29815,#29816,#29817,#29818,#29819,#29820,#29821,#29822,#29823,#29824,#29825,
#29826,#29827,#29828,#29829,#29830,#29831,#29832,#29833,#29834,#29835,#29836,
#29837,#29838,#29839,#29840,#29841,#29842,#29843,#29844,#29845,#29846,#29847,
#29848,#29849,#29850,#29851,#29852,#29853,#29854,#29855,#29856,#29857,#29858,
#29859,#29860,#29861,#29862,#29863,#29864,#29865,#29866,#29867,#29868,#29869,
#29870,#29871,#29872,#29873,#29874,#29875,#29876,#29877,#29878,#29879,#29880,
#29881,#29882,#29883,#29884,#29885,#29886,#29887,#29888,#29889,#29890,#29891,
#29892,#29893,#29894,#29895,#29896,#29897,#29898,#29899,#29900,#29901,#29902,
#29903,#29904,#29905,#29906,#29907,#29908,#29909,#29910,#29911,#29912,#29913,
#29914,#29915,#29916,#29917,#29918,#29919,#29920,#29921,#29922,#29923,#29924,
#29925,#29926,#29927,#29928,#29929,#29930,#29931,#29932,#29933,#29934,#29935,
#29936,#29937,#29938,#29939,#29940,#29941,#29942,#29943,#29944,#29945,#29946,
#29947,#29948,#29949,#29950,#29951,#29952,#29953,#29954,#29955,#29956,#29957,
#29958,#29959,#29960,#29961,#29962,#29963,#29964,#29965,#29966,#29967,#29968,
#29969,#29970,#29971,#29972,#29973,#29974,#29975,#29976,#29977,#29978,#29979,
#29980,#29981,#29982,#29983,#29984,#29985,#29986,#29987,#29988,#29989,#29990,
#29991,#29992,#29993,#29994,#29995,#29996,#29997,#29998,#29999),
 .UNSPECIFIED.,.F.,.F.,(4,3,3,3,3,3,3,3,3,3,3,3,3,3,3,3,3,3,3,3,3,3,3,3,
3,3,3,3,3,3,3,3,3,3,3,3,3,3,3,3,3,3,3,3,3,3,3,3,3,3,3,3,3,3,3,3,3,3,3,3,
3,3,3,3,3,3,3,3,3,3,3,3,3,3,3,3,3,3,3,3,3,3,3,3,3,3,3,3,3,3,3,3,3,3,3,3,
3,3,3,3,3,3,3,3,3,3,3,3,3,3,3,3,3,3,3,3,3,3,4),(0.00557323536012404,0.00813317970068968,
0.00899310447168613,0.00899708454320929,0.0121711318036108,0.0124129735832482,
0.0124180817258657,0.0155952691298109,0.0158328426948103,0.0158371230923959,
0.0192527118063724,0.0192553994766634,0.0260908370914267,0.0260924500294965,
0.0329251951059827,0.0329321882526206,0.0397587811276712,0.0397719264757448,
0.0431753551494948,0.0431917955873068,0.0465918925264685,0.0466116646988689,
0.0602580243360313,0.0602911411451171,0.0739241399711004,0.0739706175913654,
0.0875902510252554,0.0876500940376136,0.0910067777520482,0.0910699631491756,
0.0944233074266285,0.0944898322607377,0.101256366068591,0.101329570483862,
0.114922493436243,0.11500904693011,0.128588631762366,0.128688523376358,
0.13542170232537,0.135528261599482,0.138838233799944,0.138948130711044,
0.142254772288456,0.142367999822606,0.155921036358478,0.156047476268855,
0.169587707753517,0.169726952715103,0.176421304432259,0.18325516671409,
0.183406429161351,0.186672225782196,0.186826298272913,0.190089514568395,
0.190246167384475,0.194686066878316,0.19692659272522,0.197085905607599,
0.19994345888875,0.200346901177744,0.200505774719161,0.203140343629623,
0.203768953747021,0.203925643830723,0.205275623472084,0.205480868880759,
0.205635578386504,0.206726606049008,0.207193774472377,0.207345512942285,
0.208386484884662,0.208908899872059,0.209055447498066,0.209841495103125,
0.210571007656769,0.210627542708183,0.210765382053847,0.211254417816863,
0.211488962777378,0.211620349331738,0.212183813013997,0.212352708772903,
0.212475316609628,0.212785889588788,0.213193811336146,0.213220178090878,
0.213330283887519,0.213581340987045,0.213655668182996,0.213757767526464,
0.213985258897261,0.214092652619984,0.214185251165409,0.214421594048797,
0.21453045366287,0.214612734804355,0.214839128215605,0.214968872499077,
0.2150402184433,0.215406642448134,0.215753074760998,0.215843362999165,0.21589518572119,
0.21651084508489,0.216712652071532,0.216750152999081,0.217427362517899,
0.217577731954515,0.217605120276971,0.218159809721273,0.218439895499696,
0.218460087554862,0.219300288731891,0.219315054832752,0.220437296311934,
0.221017808849557,0.221024989388533,0.222735034793048,0.224444858500095),
 .UNSPECIFIED.);
#1118=B_SPLINE_CURVE_WITH_KNOTS('',3,(#30739,#30740,#30741,#30742,#30743,
#30744),.UNSPECIFIED.,.F.,.F.,(4,2,4),(-0.791676148264701,-0.372293977343492,
-9.65154153425599E-5),.UNSPECIFIED.);
#1119=B_SPLINE_CURVE_WITH_KNOTS('',3,(#30746,#30747,#30748,#30749,#30750,
#30751),.UNSPECIFIED.,.F.,.F.,(4,2,4),(1.00000001008845E-6,0.394087848699293,
0.7875399240535),.UNSPECIFIED.);
#1120=B_SPLINE_CURVE_WITH_KNOTS('',3,(#30769,#30770,#30771,#30772,#30773,
#30774),.UNSPECIFIED.,.F.,.F.,(4,2,4),(-1.2607282506686,-0.589657089902255,
-9.99999981265987E-7),.UNSPECIFIED.);
#1121=B_SPLINE_CURVE_WITH_KNOTS('',3,(#30776,#30777,#30778,#30779,#30780,
#30781),.UNSPECIFIED.,.F.,.F.,(4,2,4),(-1.20095340635985,-0.611306024392865,
-9.99999999029555E-7),.UNSPECIFIED.);
#1122=B_SPLINE_CURVE_WITH_KNOTS('',3,(#30782,#30783,#30784,#30785,#30786,
#30787),.UNSPECIFIED.,.F.,.F.,(4,2,4),(-1.38009654873525,-0.740783265368206,
-9.99999862293069E-7),.UNSPECIFIED.);
#1123=B_SPLINE_CURVE_WITH_KNOTS('',3,(#30835,#30836,#30837,#30838),
 .UNSPECIFIED.,.F.,.F.,(4,4),(-1.5577837123075,-1.08255868409364),
 .UNSPECIFIED.);
#1124=B_SPLINE_CURVE_WITH_KNOTS('',3,(#30841,#30842,#30843,#30844),
 .UNSPECIFIED.,.F.,.F.,(4,4),(-4.8771663186696,-4.4074212598598),
 .UNSPECIFIED.);
#1125=B_SPLINE_CURVE_WITH_KNOTS('',3,(#30850,#30851,#30852,#30853,#30854,
#30855,#30856,#30857),.UNSPECIFIED.,.F.,.F.,(4,2,2,4),(1.10266399002091,
1.49973808840737,2.99947617681474,3.96838445098593),.UNSPECIFIED.);
#1126=B_SPLINE_CURVE_WITH_KNOTS('',3,(#30861,#30862,#30863,#30864),
 .UNSPECIFIED.,.F.,.F.,(4,4),(3.95502240653836,4.90059859273432),
 .UNSPECIFIED.);
#1127=B_SPLINE_CURVE_WITH_KNOTS('',3,(#30868,#30869,#30870,#30871,#30872,
#30873),.UNSPECIFIED.,.F.,.F.,(4,2,4),(1.55848971014011,2.98315547534721,
4.87725449444892),.UNSPECIFIED.);
#1128=B_SPLINE_CURVE_WITH_KNOTS('',3,(#30878,#30879,#30880,#30881),
 .UNSPECIFIED.,.F.,.F.,(4,4),(-2.02935178929506,-1.08377694268274),
 .UNSPECIFIED.);
#1129=B_SPLINE_CURVE_WITH_KNOTS('',3,(#30895,#30896,#30897,#30898,#30899,
#30900),.UNSPECIFIED.,.F.,.F.,(4,2,4),(1.27063161726614,1.45139131523522,
1.5474010823708),.UNSPECIFIED.);
#1130=B_SPLINE_CURVE_WITH_KNOTS('',3,(#30904,#30905,#30906,#30907,#30908,
#30909),.UNSPECIFIED.,.F.,.F.,(4,2,4),(2.04697459142689,2.07719778912169,
2.13306764446534),.UNSPECIFIED.);
#1131=B_SPLINE_CURVE_WITH_KNOTS('',3,(#30913,#30914,#30915,#30916,#30917,
#30918),.UNSPECIFIED.,.F.,.F.,(4,2,4),(4.13426269446195,4.1901325498056,
4.22035574750039),.UNSPECIFIED.);
#1132=B_SPLINE_CURVE_WITH_KNOTS('',3,(#30921,#30922,#30923,#30924,#30925,
#30926),.UNSPECIFIED.,.F.,.F.,(4,2,4),(0.993862152161476,1.08987191929705,
1.27063161726614),.UNSPECIFIED.);
#1133=B_SPLINE_CURVE_WITH_KNOTS('',3,(#30956,#30957,#30958,#30959,#30960,
#30961,#30962,#30963,#30964,#30965,#30966,#30967,#30968,#30969,#30970,#30971,
#30972,#30973),.UNSPECIFIED.,.F.,.F.,(4,2,2,2,2,2,2,2,4),(-1.27702533132968,
-1.25572868727499,-1.16995330406695,-0.996929092471484,-0.823904880876014,
-0.650880669280543,-0.477856457685072,-0.392081074477042,-0.370784430421933),
 .UNSPECIFIED.);
#1134=B_SPLINE_CURVE_WITH_KNOTS('',3,(#30977,#30978,#30979,#30980,#30981,
#30982,#30983,#30984,#30985,#30986,#30987,#30988,#30989,#30990,#30991,#30992,
#30993,#30994),.UNSPECIFIED.,.F.,.F.,(4,2,2,2,2,2,2,2,4),(-2.9248350930817,
-2.90353844902701,-2.81776306581898,-2.64473885422351,-2.47171464262804,
-2.29869043103257,-2.1256662194371,-2.03989083622907,-2.01859419217395),
 .UNSPECIFIED.);
#1135=B_SPLINE_CURVE_WITH_KNOTS('',3,(#30999,#31000,#31001,#31002,#31003,
#31004,#31005,#31006,#31007,#31008,#31009,#31010,#31011,#31012,#31013,#31014,
#31015,#31016),.UNSPECIFIED.,.F.,.F.,(4,2,2,2,2,2,2,2,4),(-1.27702533132966,
-1.25572868727497,-1.16995330406694,-0.996929092471472,-0.823904880876004,
-0.650880669280535,-0.477856457685067,-0.392081074477038,-0.370784430421922),
 .UNSPECIFIED.);
#1136=B_SPLINE_CURVE_WITH_KNOTS('',3,(#31020,#31021,#31022,#31023,#31024,
#31025,#31026,#31027,#31028,#31029,#31030,#31031,#31032,#31033,#31034,#31035,
#31036,#31037),.UNSPECIFIED.,.F.,.F.,(4,2,2,2,2,2,2,2,4),(-2.92483509308168,
-2.90353844902699,-2.81776306581896,-2.64473885422349,-2.47171464262802,
-2.29869043103255,-2.12566621943708,-2.03989083622905,-2.01859419217394),
 .UNSPECIFIED.);
#1137=B_SPLINE_CURVE_WITH_KNOTS('',3,(#31044,#31045,#31046,#31047,#31048,
#31049),.UNSPECIFIED.,.F.,.F.,(4,2,4),(1.49165309308059,1.52025985898216,
1.82900497420274),.UNSPECIFIED.);
#1138=B_SPLINE_CURVE_WITH_KNOTS('',3,(#31053,#31054,#31055,#31056,#31057,
#31058),.UNSPECIFIED.,.F.,.F.,(4,2,4),(2.83826458115358,3.14700969637418,
3.17561646227572),.UNSPECIFIED.);
#1139=B_SPLINE_CURVE_WITH_KNOTS('',3,(#31062,#31063,#31064,#31065,#31066,
#31067,#31068,#31069),.UNSPECIFIED.,.F.,.F.,(4,2,2,4),(2.01859419217413,
2.03989083622903,2.12566621943706,2.2046980767185),.UNSPECIFIED.);
#1140=B_SPLINE_CURVE_WITH_KNOTS('',3,(#31072,#31073,#31074,#31075,#31076,
#31077,#31078,#31079),.UNSPECIFIED.,.F.,.F.,(4,2,2,4),(1.09092144678542,
1.16995330406693,1.25572868727496,1.27702533132984),.UNSPECIFIED.);
#1141=B_SPLINE_CURVE_WITH_KNOTS('',3,(#31083,#31084,#31085,#31086,#31087,
#31088,#31089,#31090,#31091,#31092,#31093,#31094,#31095,#31096,#31097,#31098,
#31099,#31100),.UNSPECIFIED.,.F.,.F.,(4,2,2,2,2,2,2,2,4),(-1.27702533132966,
-1.25572868727498,-1.16995330406695,-0.996929092471477,-0.823904880876007,
-0.650880669280538,-0.477856457685069,-0.392081074477039,-0.370784430421927),
 .UNSPECIFIED.);
#1142=B_SPLINE_CURVE_WITH_KNOTS('',3,(#31109,#31110,#31111,#31112,#31113,
#31114,#31115,#31116,#31117,#31118,#31119,#31120,#31121,#31122,#31123,#31124,
#31125,#31126),.UNSPECIFIED.,.F.,.F.,(4,2,2,2,2,2,2,2,4),(-1.27702533132965,
-1.25572868727496,-1.16995330406693,-0.99692909247146,-0.823904880875993,
-0.650880669280526,-0.47785645768506,-0.392081074477032,-0.370784430421916),
 .UNSPECIFIED.);
#1143=B_SPLINE_CURVE_WITH_KNOTS('',3,(#31130,#31131,#31132,#31133,#31134,
#31135,#31136,#31137,#31138,#31139,#31140,#31141,#31142,#31143,#31144,#31145,
#31146,#31147),.UNSPECIFIED.,.F.,.F.,(4,2,2,2,2,2,2,2,4),(-2.92483509308164,
-2.90353844902695,-2.81776306581892,-2.64473885422345,-2.47171464262799,
-2.29869043103252,-2.12566621943705,-2.03989083622902,-2.0185941921739),
 .UNSPECIFIED.);
#1144=B_SPLINE_CURVE_WITH_KNOTS('',3,(#31197,#31198,#31199,#31200,#31201,
#31202,#31203,#31204,#31205,#31206,#31207,#31208,#31209,#31210,#31211,#31212,
#31213,#31214),.UNSPECIFIED.,.F.,.F.,(4,2,2,2,2,2,2,2,4),(-2.92483509308168,
-2.90353844902699,-2.81776306581896,-2.64473885422349,-2.47171464262802,
-2.29869043103255,-2.12566621943708,-2.03989083622905,-2.01859419217394),
 .UNSPECIFIED.);
#1145=B_SPLINE_CURVE_WITH_KNOTS('',3,(#31223,#31224,#31225,#31226,#31227,
#31228,#31229,#31230,#31231,#31232),.UNSPECIFIED.,.F.,.F.,(4,2,2,2,4),(0.500868628985409,
0.735493341191987,0.896904927369324,1.05831651354666,1.26986694206134),
 .UNSPECIFIED.);
#1146=B_SPLINE_CURVE_WITH_KNOTS('',3,(#31233,#31234,#31235,#31236,#31237,
#31238,#31239,#31240,#31241,#31242),.UNSPECIFIED.,.F.,.F.,(4,2,2,2,4),(1.6584322305039,
1.91496011666266,2.10521778038795,2.29547544411323,2.60768377754927),
 .UNSPECIFIED.);
#1147=B_SPLINE_CURVE_WITH_KNOTS('',3,(#31252,#31253,#31254,#31255,#31256,
#31257,#31258,#31259,#31260,#31261,#31262,#31263),.UNSPECIFIED.,.F.,.F.,
(4,2,2,2,2,4),(-2.23899247185989,-2.23353118304087,-1.98720488286121,-1.74087858268154,
-1.48331632361342,-1.47375923154499),.UNSPECIFIED.);
#1148=B_SPLINE_CURVE_WITH_KNOTS('',3,(#31330,#31331,#31332,#31333,#31334,
#31335,#31336,#31337,#31338,#31339,#31340,#31341,#31342,#31343,#31344,#31345,
#31346,#31347,#31348,#31349,#31350,#31351,#31352,#31353),.UNSPECIFIED.,
 .F.,.F.,(4,2,2,2,2,2,2,2,2,2,2,4),(3.54201414503647,3.60917199339226,3.64693471091968,
3.6846974284471,3.70035540208751,3.71601337572793,3.7335287617438,3.75104414775967,
3.78450531236555,3.81796647697143,3.88488880618319,3.9103123168716),
 .UNSPECIFIED.);
#1149=B_SPLINE_CURVE_WITH_KNOTS('',3,(#31354,#31355,#31356,#31357,#31358,
#31359),.UNSPECIFIED.,.F.,.F.,(4,2,4),(-16.2126008937337,-16.1073352653066,
-15.971670557086),.UNSPECIFIED.);
#1150=B_SPLINE_CURVE_WITH_KNOTS('',3,(#31532,#31533,#31534,#31535,#31536,
#31537,#31538,#31539,#31540,#31541),.UNSPECIFIED.,.F.,.F.,(4,2,2,2,4),(0.,
0.223184802145918,0.439747194735359,0.656355638915093,0.879587963358382),
 .UNSPECIFIED.);
#1151=B_SPLINE_CURVE_WITH_KNOTS('',3,(#31543,#31544,#31545,#31546,#31547,
#31548),.UNSPECIFIED.,.F.,.F.,(4,2,4),(0.,0.160388841871916,0.315547520092146),
 .UNSPECIFIED.);
#1152=B_SPLINE_CURVE_WITH_KNOTS('',3,(#31552,#31553,#31554,#31555,#31556,
#31557),.UNSPECIFIED.,.F.,.F.,(4,2,4),(0.,0.151579443123173,0.307260734801231),
 .UNSPECIFIED.);
#1153=B_SPLINE_CURVE_WITH_KNOTS('',3,(#31559,#31560,#31561,#31562,#31563,
#31564,#31565,#31566,#31567,#31568),.UNSPECIFIED.,.F.,.F.,(4,2,2,2,4),(0.,
0.212152978397668,0.422051181763095,0.652730480685441,0.893650672439128),
 .UNSPECIFIED.);
#1154=B_SPLINE_CURVE_WITH_KNOTS('',3,(#31570,#31571,#31572,#31573,#31574,
#31575),.UNSPECIFIED.,.F.,.F.,(4,2,4),(0.,0.143871076035642,0.282736346863713),
 .UNSPECIFIED.);
#1155=B_SPLINE_CURVE_WITH_KNOTS('',3,(#31579,#31580,#31581,#31582,#31583,
#31584),.UNSPECIFIED.,.F.,.F.,(4,2,4),(0.,0.276923219658822,0.495895501945399),
 .UNSPECIFIED.);
#1156=B_SPLINE_CURVE_WITH_KNOTS('',3,(#31586,#31587,#31588,#31589,#31590,
#31591),.UNSPECIFIED.,.F.,.F.,(4,2,4),(-1.31438656188044,-0.675941586797486,
0.),.UNSPECIFIED.);
#1157=B_SPLINE_CURVE_WITH_KNOTS('',3,(#31599,#31600,#31601,#31602,#31603,
#31604),.UNSPECIFIED.,.F.,.F.,(4,2,4),(-1.31452379814346,-0.638512700577341,
-9.87344898062403E-7),.UNSPECIFIED.);
#1158=B_SPLINE_CURVE_WITH_KNOTS('',3,(#31606,#31607,#31608,#31609,#31610,
#31611),.UNSPECIFIED.,.F.,.F.,(4,2,4),(1.00970274276848E-6,0.207625682362454,
0.496418277299487),.UNSPECIFIED.);
#1159=B_SPLINE_CURVE_WITH_KNOTS('',3,(#31615,#31616,#31617,#31618,#31619,
#31620),.UNSPECIFIED.,.F.,.F.,(4,2,4),(1.00000002999262E-6,0.159334194743211,
0.282730318724299),.UNSPECIFIED.);
#1160=B_SPLINE_CURVE_WITH_KNOTS('',3,(#31622,#31623,#31624,#31625,#31626,
#31627,#31628,#31629),.UNSPECIFIED.,.F.,.F.,(4,2,2,4),(0.,0.414719851775387,
0.654098578320246,0.895378619929204),.UNSPECIFIED.);
#1161=B_SPLINE_CURVE_WITH_KNOTS('',3,(#31631,#31632,#31633,#31634,#31635,
#31636),.UNSPECIFIED.,.F.,.F.,(4,2,4),(0.,0.155726590263008,0.307315201685305),
 .UNSPECIFIED.);
#1162=B_SPLINE_CURVE_WITH_KNOTS('',3,(#31639,#31640,#31641,#31642,#31643,
#31644),.UNSPECIFIED.,.F.,.F.,(4,2,4),(0.,0.155122646177725,0.315476068796403),
 .UNSPECIFIED.);
#1163=B_SPLINE_CURVE_WITH_KNOTS('',3,(#31692,#31693,#31694,#31695,#31696,
#31697,#31698,#31699),.UNSPECIFIED.,.F.,.F.,(4,2,2,4),(-1.20146899372566,
-0.600846725288746,-0.240887418321441,0.),.UNSPECIFIED.);
#1164=B_SPLINE_CURVE_WITH_KNOTS('',3,(#31709,#31710,#31711,#31712,#31713,
#31714,#31715,#31716,#31717,#31718,#31719,#31720),.UNSPECIFIED.,.F.,.F.,
(4,2,2,2,2,4),(-1.49738934525104,-1.30249117565947,-1.11538918315606,-0.877104450222815,
-0.53567900892061,0.),.UNSPECIFIED.);
#1165=B_SPLINE_CURVE_WITH_KNOTS('',3,(#31732,#31733,#31734,#31735,#31736,
#31737,#31738,#31739,#31740,#31741,#31742,#31743,#31744,#31745,#31746,#31747,
#31748,#31749,#31750,#31751,#31752,#31753,#31754,#31755,#31756,#31757,#31758,
#31759,#31760,#31761,#31762,#31763,#31764,#31765),.UNSPECIFIED.,.F.,.F.,
(4,3,3,3,3,3,3,3,3,3,3,4),(0.0428656554157575,0.13679913434849,0.230446688335681,
0.326640852293718,0.419914650723107,0.513145592287718,0.606396601892675,
0.699730411778525,0.793321120935319,0.887097673400666,0.981233417826358,
0.999999999999973),.UNSPECIFIED.);
#1166=B_SPLINE_CURVE_WITH_KNOTS('',3,(#31766,#31767,#31768,#31769,#31770,
#31771),.UNSPECIFIED.,.F.,.F.,(4,2,4),(-0.981740143086555,-0.521961463111386,
0.),.UNSPECIFIED.);
#1167=B_SPLINE_CURVE_WITH_KNOTS('',3,(#31787,#31788,#31789,#31790,#31791,
#31792),.UNSPECIFIED.,.F.,.F.,(4,2,4),(-0.133416986009087,-0.0667110879136702,
-5.1910372269785E-6),.UNSPECIFIED.);
#1168=B_SPLINE_CURVE_WITH_KNOTS('',3,(#31805,#31806,#31807,#31808,#31809,
#31810),.UNSPECIFIED.,.F.,.F.,(4,2,4),(9.99999978184638E-7,0.649745648357186,
1.35925358102172),.UNSPECIFIED.);
#1169=B_SPLINE_CURVE_WITH_KNOTS('',3,(#31812,#31813,#31814,#31815,#31816,
#31817),.UNSPECIFIED.,.F.,.F.,(4,2,4),(0.,0.394929358834096,0.789859724379243),
 .UNSPECIFIED.);
#1170=B_SPLINE_CURVE_WITH_KNOTS('',3,(#31819,#31820,#31821,#31822,#31823,
#31824),.UNSPECIFIED.,.F.,.F.,(4,2,4),(-0.203128010071857,-0.10156462327841,
-1.00000000322065E-6),.UNSPECIFIED.);
#1171=B_SPLINE_CURVE_WITH_KNOTS('',3,(#31825,#31826,#31827,#31828,#31829,
#31830),.UNSPECIFIED.,.F.,.F.,(4,2,4),(1.49144212074817,1.98945111447353,
2.50597513326044),.UNSPECIFIED.);
#1172=B_SPLINE_CURVE_WITH_KNOTS('',3,(#31841,#31842,#31843,#31844,#31845,
#31846,#31847,#31848,#31849,#31850,#31851,#31852),.UNSPECIFIED.,.F.,.F.,
(4,2,2,2,2,4),(-1.49732839853819,-0.998653556005853,-0.620289629858932,
-0.365781376210274,-0.185635579466019,0.),.UNSPECIFIED.);
#1173=B_SPLINE_CURVE_WITH_KNOTS('',3,(#31866,#31867,#31868,#31869,#31870,
#31871),.UNSPECIFIED.,.F.,.F.,(4,2,4),(-0.991698835186327,-0.464861205496753,
0.),.UNSPECIFIED.);
#1174=B_SPLINE_CURVE_WITH_KNOTS('',3,(#31872,#31873,#31874,#31875,#31876,
#31877,#31878,#31879,#31880,#31881,#31882,#31883,#31884,#31885,#31886,#31887,
#31888,#31889,#31890,#31891,#31892,#31893,#31894,#31895,#31896,#31897,#31898,
#31899,#31900,#31901,#31902,#31903,#31904,#31905),.UNSPECIFIED.,.F.,.F.,
(4,3,3,3,3,3,3,3,3,3,3,4),(1.80628081936085E-16,0.0941353335519054,0.187946410909733,
0.284092730197232,0.377429083695201,0.470683798845207,0.563919701125802,
0.657199745463011,0.750681328969369,0.844317073902783,0.938269188721954,
0.957116965209728),.UNSPECIFIED.);
#1175=B_SPLINE_CURVE_WITH_KNOTS('',3,(#31917,#31918,#31919,#31920,#31921,
#31922,#31923,#31924,#31925,#31926),.UNSPECIFIED.,.F.,.F.,(4,2,2,2,4),(-1.49714596644318,
-1.13508004089971,-0.778547165757211,-0.375322448427936,0.),
 .UNSPECIFIED.);
#1176=B_SPLINE_CURVE_WITH_KNOTS('',3,(#31940,#31941,#31942,#31943,#31944,
#31945,#31946,#31947,#31948,#31949,#31950,#31951,#31952,#31953,#31954,#31955,
#31956,#31957,#31958,#31959,#31960,#31961,#31962,#31963,#31964,#31965,#31966,
#31967,#31968,#31969,#31970,#31971,#31972,#31973),.UNSPECIFIED.,.F.,.F.,
(4,3,3,3,3,3,3,3,3,3,3,4),(0.0426189802653293,0.136532611271545,0.230169834401958,
0.326398605101725,0.41967855846039,0.512918289440782,0.606178554076897,
0.699519886497026,0.793111915273064,0.886884192924315,0.9810061634702,1.00000000000009),
 .UNSPECIFIED.);
#1177=B_SPLINE_CURVE_WITH_KNOTS('',3,(#31974,#31975,#31976,#31977,#31978,
#31979),.UNSPECIFIED.,.F.,.F.,(4,2,4),(-0.970835171563933,-0.515920953006016,
0.),.UNSPECIFIED.);
#1178=B_SPLINE_CURVE_WITH_KNOTS('',3,(#31991,#31992,#31993,#31994,#31995,
#31996,#31997,#31998,#31999,#32000),.UNSPECIFIED.,.F.,.F.,(4,2,2,2,4),(-1.49810739332486,
-1.34911047074889,-0.620300163072249,-0.284723572909162,0.),
 .UNSPECIFIED.);
#1179=B_SPLINE_CURVE_WITH_KNOTS('',3,(#32012,#32013,#32014,#32015,#32016,
#32017,#32018,#32019,#32020,#32021),.UNSPECIFIED.,.F.,.F.,(4,2,2,2,4),(-1.49747557017719,
-1.09769840149384,-0.714928203148522,-0.377751581416893,0.),
 .UNSPECIFIED.);
#1180=B_SPLINE_CURVE_WITH_KNOTS('',3,(#32472,#32473,#32474,#32475,#32476,
#32477),.UNSPECIFIED.,.F.,.F.,(4,2,4),(-0.981606280218853,-0.521850501049393,
0.),.UNSPECIFIED.);
#1181=B_SPLINE_CURVE_WITH_KNOTS('',3,(#32482,#32483,#32484,#32485,#32486,
#32487),.UNSPECIFIED.,.F.,.F.,(4,2,4),(-1.26025824344159,-0.587863989490026,
-9.99999988926525E-7),.UNSPECIFIED.);
#1182=B_SPLINE_CURVE_WITH_KNOTS('',3,(#32493,#32494,#32495,#32496,#32497,
#32498),.UNSPECIFIED.,.F.,.F.,(4,2,4),(-1.20095164808206,-0.601230313153804,
-9.9999999636502E-7),.UNSPECIFIED.);
#1183=B_SPLINE_CURVE_WITH_KNOTS('',3,(#32503,#32504,#32505,#32506,#32507,
#32508),.UNSPECIFIED.,.F.,.F.,(4,2,4),(-0.979787980011625,-0.459672473975673,
0.),.UNSPECIFIED.);
#1184=B_SPLINE_CURVE_WITH_KNOTS('',3,(#32509,#32510,#32511,#32512,#32513,
#32514),.UNSPECIFIED.,.F.,.F.,(4,2,4),(-1.20447770770638,-0.642888512151301,
-9.99999843598331E-7),.UNSPECIFIED.);
#1185=B_SPLINE_CURVE_WITH_KNOTS('',3,(#32520,#32521,#32522,#32523,#32524,
#32525),.UNSPECIFIED.,.F.,.F.,(4,2,4),(-1.27174362759288,-0.592870374348338,
-9.99999989116678E-7),.UNSPECIFIED.);
#1186=B_SPLINE_CURVE_WITH_KNOTS('',3,(#32531,#32532,#32533,#32534,#32535,
#32536),.UNSPECIFIED.,.F.,.F.,(4,2,4),(-1.20095492134397,-0.600247667823548,
-9.99999999029555E-7),.UNSPECIFIED.);
#1187=B_SPLINE_CURVE_WITH_KNOTS('',3,(#32538,#32539,#32540,#32541,#32542,
#32543),.UNSPECIFIED.,.F.,.F.,(4,2,4),(-1.1923457836634,-0.636112763433397,
-9.9999983627086E-7),.UNSPECIFIED.);
#1188=B_SPLINE_CURVE_WITH_KNOTS('',3,(#32558,#32559,#32560,#32561,#32562,
#32563,#32564,#32565,#32566,#32567),.UNSPECIFIED.,.F.,.F.,(4,2,2,2,4),(-0.811018179914924,
-0.664454692598758,-0.572774590965832,-0.394840790088965,0.),
 .UNSPECIFIED.);
#1189=B_SPLINE_CURVE_WITH_KNOTS('',3,(#32572,#32573,#32574,#32575,#32576,
#32577),.UNSPECIFIED.,.F.,.F.,(4,2,4),(-1.46761581044962,-0.679870711727504,
-9.99999985706879E-7),.UNSPECIFIED.);
#1190=B_SPLINE_CURVE_WITH_KNOTS('',3,(#32583,#32584,#32585,#32586,#32587,
#32588),.UNSPECIFIED.,.F.,.F.,(4,2,4),(-1.20095336165845,-0.589756404209531,
-9.99999999465967E-7),.UNSPECIFIED.);
#1191=B_SPLINE_CURVE_WITH_KNOTS('',3,(#32591,#32592,#32593,#32594,#32595,
#32596),.UNSPECIFIED.,.F.,.F.,(4,2,4),(-1.25535652774483,-0.666244907753614,
-1.33226762955019E-15),.UNSPECIFIED.);
#1192=B_SPLINE_CURVE_WITH_KNOTS('',3,(#32599,#32600,#32601,#32602,#32603,
#32604),.UNSPECIFIED.,.F.,.F.,(4,2,4),(-0.990141997994943,-0.466167882443553,
-9.99999943980542E-7),.UNSPECIFIED.);
#1193=B_SPLINE_CURVE_WITH_KNOTS('',3,(#32608,#32609,#32610,#32611,#32612,
#32613,#32614,#32615),.UNSPECIFIED.,.F.,.F.,(4,2,2,4),(9.99977311176857E-7,
0.108585823432627,0.151061815337212,0.21421875376243),.UNSPECIFIED.);
#1194=B_SPLINE_CURVE_WITH_KNOTS('',3,(#32619,#32620,#32621,#32622,#32623,
#32624),.UNSPECIFIED.,.F.,.F.,(4,2,4),(0.,0.393385683687471,0.787575248868537),
 .UNSPECIFIED.);
#1195=B_SPLINE_CURVE_WITH_KNOTS('',3,(#32628,#32629,#32630,#32631,#32632,
#32633),.UNSPECIFIED.,.F.,.F.,(4,2,4),(1.00000001804486E-6,0.394931365545149,
0.789860724379214),.UNSPECIFIED.);
#1196=B_SPLINE_CURVE_WITH_KNOTS('',3,(#32635,#32636,#32637,#32638,#32639,
#32640),.UNSPECIFIED.,.F.,.F.,(4,2,4),(0.,0.399659978932644,0.799320001325682),
 .UNSPECIFIED.);
#1197=B_SPLINE_CURVE_WITH_KNOTS('',3,(#32642,#32643,#32644,#32645,#32646,
#32647),.UNSPECIFIED.,.F.,.F.,(4,2,4),(0.,0.333003326126868,0.666006652253743),
 .UNSPECIFIED.);
#1198=B_SPLINE_CURVE_WITH_KNOTS('',3,(#32649,#32650,#32651,#32652,#32653,
#32654),.UNSPECIFIED.,.F.,.F.,(4,2,4),(0.,0.396114271378094,0.792228542747862),
 .UNSPECIFIED.);
#1199=B_SPLINE_CURVE_WITH_KNOTS('',3,(#32656,#32657,#32658,#32659,#32660,
#32661),.UNSPECIFIED.,.F.,.F.,(4,2,4),(0.,0.333003326126872,0.666006652253742),
 .UNSPECIFIED.);
#1200=B_SPLINE_CURVE_WITH_KNOTS('',3,(#32662,#32663,#32664,#32665,#32666,
#32667),.UNSPECIFIED.,.F.,.F.,(4,2,4),(0.,0.399660022402238,0.799320001325697),
 .UNSPECIFIED.);
#1201=B_SPLINE_CURVE_WITH_KNOTS('',3,(#32669,#32670,#32671,#32672,#32673,
#32674),.UNSPECIFIED.,.F.,.F.,(4,2,4),(4.61607433837006E-5,0.394237334279624,
0.787624623042523),.UNSPECIFIED.);
#1202=B_SPLINE_CURVE_WITH_KNOTS('',3,(#32675,#32676,#32677,#32678,#32679,
#32680),.UNSPECIFIED.,.F.,.F.,(4,2,4),(0.,0.393451752374059,0.78755756073778),
 .UNSPECIFIED.);
#1203=B_SPLINE_CURVE_WITH_KNOTS('',3,(#32684,#32685,#32686,#32687,#32688,
#32689),.UNSPECIFIED.,.F.,.F.,(4,2,4),(1.0000000167154E-6,0.394931365545151,
0.78986072437921),.UNSPECIFIED.);
#1204=B_SPLINE_CURVE_WITH_KNOTS('',3,(#32691,#32692,#32693,#32694,#32695,
#32696),.UNSPECIFIED.,.F.,.F.,(4,2,4),(0.,0.399659978932271,0.799320001325689),
 .UNSPECIFIED.);
#1205=B_SPLINE_CURVE_WITH_KNOTS('',3,(#32698,#32699,#32700,#32701,#32702,
#32703),.UNSPECIFIED.,.F.,.F.,(4,2,4),(0.,0.333003326126866,0.666006652253748),
 .UNSPECIFIED.);
#1206=B_SPLINE_CURVE_WITH_KNOTS('',3,(#32705,#32706,#32707,#32708,#32709,
#32710),.UNSPECIFIED.,.F.,.F.,(4,2,4),(0.,0.396114271378084,0.79222854274787),
 .UNSPECIFIED.);
#1207=B_SPLINE_CURVE_WITH_KNOTS('',3,(#32712,#32713,#32714,#32715,#32716,
#32717),.UNSPECIFIED.,.F.,.F.,(4,2,4),(0.,0.333003326126869,0.666006652253723),
 .UNSPECIFIED.);
#1208=B_SPLINE_CURVE_WITH_KNOTS('',3,(#32719,#32720,#32721,#32722,#32723,
#32724),.UNSPECIFIED.,.F.,.F.,(4,2,4),(0.,0.399660022402634,0.799320001325709),
 .UNSPECIFIED.);
#1209=B_SPLINE_CURVE_WITH_KNOTS('',3,(#32726,#32727,#32728,#32729,#32730,
#32731),.UNSPECIFIED.,.F.,.F.,(4,2,4),(0.,0.394929358834099,0.789859724379254),
 .UNSPECIFIED.);
#1210=B_SPLINE_CURVE_WITH_KNOTS('',3,(#32746,#32747,#32748,#32749,#32750,
#32751),.UNSPECIFIED.,.F.,.F.,(4,2,4),(1.00000001560095E-6,0.394931365545173,
0.789860724379263),.UNSPECIFIED.);
#1211=B_SPLINE_CURVE_WITH_KNOTS('',3,(#32753,#32754,#32755,#32756,#32757,
#32758),.UNSPECIFIED.,.F.,.F.,(4,2,4),(0.,0.399659978931984,0.799320001325694),
 .UNSPECIFIED.);
#1212=B_SPLINE_CURVE_WITH_KNOTS('',3,(#32760,#32761,#32762,#32763,#32764,
#32765),.UNSPECIFIED.,.F.,.F.,(4,2,4),(0.,0.333003326126855,0.666006652253734),
 .UNSPECIFIED.);
#1213=B_SPLINE_CURVE_WITH_KNOTS('',3,(#32767,#32768,#32769,#32770,#32771,
#32772),.UNSPECIFIED.,.F.,.F.,(4,2,4),(0.,0.396114271378083,0.792228542747862),
 .UNSPECIFIED.);
#1214=B_SPLINE_CURVE_WITH_KNOTS('',3,(#32774,#32775,#32776,#32777,#32778,
#32779),.UNSPECIFIED.,.F.,.F.,(4,2,4),(0.,0.333003326126878,0.666006652253737),
 .UNSPECIFIED.);
#1215=B_SPLINE_CURVE_WITH_KNOTS('',3,(#32781,#32782,#32783,#32784,#32785,
#32786),.UNSPECIFIED.,.F.,.F.,(4,2,4),(0.,0.399660022402913,0.79932000132569),
 .UNSPECIFIED.);
#1216=B_SPLINE_CURVE_WITH_KNOTS('',3,(#32788,#32789,#32790,#32791,#32792,
#32793),.UNSPECIFIED.,.F.,.F.,(4,2,4),(0.,0.394929358834091,0.789859724379262),
 .UNSPECIFIED.);
#1217=B_SPLINE_CURVE_WITH_KNOTS('',3,(#32796,#32797,#32798,#32799,#32800,
#32801),.UNSPECIFIED.,.F.,.F.,(4,2,4),(1.00000001065878E-6,0.393842731522518,
0.787628258068762),.UNSPECIFIED.);
#1218=B_SPLINE_CURVE_WITH_KNOTS('',3,(#32803,#32804,#32805,#32806,#32807,
#32808,#32809,#32810,#32811,#32812,#32813,#32814,#32815,#32816,#32817,#32818,
#32819,#32820,#32821,#32822,#32823,#32824,#32825,#32826,#32827,#32828,#32829),
 .UNSPECIFIED.,.F.,.F.,(4,3,3,3,3,3,2,2,2,2,4),(0.,0.166384002763973,0.200043514355487,
0.333101812640448,0.400072323934008,0.500472422318454,0.667828884642908,
0.667927982169589,0.834482890734559,0.834643736071572,0.99999999990215),
 .UNSPECIFIED.);
#1219=B_SPLINE_CURVE_WITH_KNOTS('',3,(#32833,#32834,#32835,#32836,#32837,
#32838,#32839,#32840),.UNSPECIFIED.,.F.,.F.,(4,2,2,4),(9.99976141228907E-7,
0.105157211260081,0.151172928145465,0.210254656084201),.UNSPECIFIED.);
#1220=B_SPLINE_CURVE_WITH_KNOTS('',3,(#32842,#32843,#32844,#32845,#32846,
#32847,#32848,#32849),.UNSPECIFIED.,.F.,.F.,(4,2,2,4),(9.99965210135567E-7,
0.0633219202251493,0.106228627126563,0.154610242485071),.UNSPECIFIED.);
#1221=B_SPLINE_CURVE_WITH_KNOTS('',3,(#32851,#32852,#32853,#32854,#32855,
#32856),.UNSPECIFIED.,.F.,.F.,(4,2,4),(9.99965276140573E-7,0.0775123835625057,
0.155023767084188),.UNSPECIFIED.);
#1222=B_SPLINE_CURVE_WITH_KNOTS('',3,(#32858,#32859,#32860,#32861,#32862,
#32863,#32864,#32865),.UNSPECIFIED.,.F.,.F.,(4,2,2,4),(9.99966295642252E-7,
0.0658748368226187,0.110565073148263,0.160346982706108),.UNSPECIFIED.);
#1223=B_SPLINE_CURVE_WITH_KNOTS('',3,(#32867,#32868,#32869,#32870,#32871,
#32872),.UNSPECIFIED.,.F.,.F.,(4,2,4),(9.99986040324985E-7,0.164974177883319,
0.361524612017389),.UNSPECIFIED.);
#1224=B_SPLINE_CURVE_WITH_KNOTS('',3,(#32873,#32874,#32875,#32876,#32877,
#32878,#32879,#32880),.UNSPECIFIED.,.F.,.F.,(4,2,2,4),(9.9999999975075E-7,
0.128289718374617,0.220416183775122,0.361296752356353),.UNSPECIFIED.);
#1225=B_SPLINE_CURVE_WITH_KNOTS('',3,(#32967,#32968,#32969,#32970,#32971,
#32972,#32973,#32974,#32975,#32976,#32977,#32978,#32979,#32980,#32981,#32982,
#32983,#32984,#32985,#32986,#32987,#32988,#32989,#32990,#32991,#32992),
 .UNSPECIFIED.,.F.,.F.,(4,2,2,2,2,2,2,2,2,2,2,2,4),(-0.668077385109111,
-0.655486882058708,-0.645122638439435,-0.624392837944345,-0.58292822337847,
-0.499980909052796,-0.334030281527956,-0.168124054836522,-0.0851704516733711,
-0.0436954289381117,-0.0229585825929834,-0.0125903518508265,-9.99972897337794E-7),
 .UNSPECIFIED.);
#1226=B_SPLINE_CURVE_WITH_KNOTS('',3,(#33019,#33020,#33021,#33022,#33023,
#33024,#33025,#33026),.UNSPECIFIED.,.F.,.F.,(4,2,2,4),(9.99999997781767E-7,
1.05861232407444,1.79204764279102,2.50572967370245),.UNSPECIFIED.);
#1227=B_SPLINE_CURVE_WITH_KNOTS('',3,(#33027,#33028,#33029,#33030,#33031,
#33032),.UNSPECIFIED.,.F.,.F.,(4,2,4),(-1.31283511954368,-0.637662453649952,
-9.87368154348189E-7),.UNSPECIFIED.);
#1228=B_SPLINE_CURVE_WITH_KNOTS('',3,(#33037,#33038,#33039,#33040,#33041,
#33042),.UNSPECIFIED.,.F.,.F.,(4,2,4),(-0.219238344309207,-0.109619779347491,
-1.00000000258227E-6),.UNSPECIFIED.);
#1229=B_SPLINE_CURVE_WITH_KNOTS('',3,(#33051,#33052,#33053,#33054,#33055,
#33056),.UNSPECIFIED.,.F.,.F.,(4,2,4),(1.0096733036915E-6,0.204604110997339,
0.489538124307061),.UNSPECIFIED.);
#1230=B_SPLINE_CURVE_WITH_KNOTS('',3,(#33059,#33060,#33061,#33062,#33063,
#33064),.UNSPECIFIED.,.F.,.F.,(4,2,4),(1.00000037364389E-6,0.154897514630139,
0.274475905655399),.UNSPECIFIED.);
#1231=B_SPLINE_CURVE_WITH_KNOTS('',3,(#33075,#33076,#33077,#33078,#33079,
#33080,#33081,#33082),.UNSPECIFIED.,.F.,.F.,(4,2,2,4),(0.,0.414903698568167,
0.654288803333593,0.895643214275791),.UNSPECIFIED.);
#1232=B_SPLINE_CURVE_WITH_KNOTS('',3,(#33087,#33088,#33089,#33090,#33091,
#33092),.UNSPECIFIED.,.F.,.F.,(4,2,4),(-0.236447866929972,-0.118098613922891,
0.),.UNSPECIFIED.);
#1233=B_SPLINE_CURVE_WITH_KNOTS('',3,(#33103,#33104,#33105,#33106,#33107,
#33108),.UNSPECIFIED.,.F.,.F.,(4,2,4),(0.,0.150850161004902,0.306679145643486),
 .UNSPECIFIED.);
#1234=B_SPLINE_CURVE_WITH_KNOTS('',3,(#33109,#33110,#33111,#33112,#33113,
#33114),.UNSPECIFIED.,.F.,.F.,(4,2,4),(0.,0.151283693630131,0.298616647391532),
 .UNSPECIFIED.);
#1235=B_SPLINE_CURVE_WITH_KNOTS('',3,(#33125,#33126,#33127,#33128,#33129,
#33130,#33131,#33132,#33133,#33134),.UNSPECIFIED.,.F.,.F.,(4,2,2,2,4),(-0.879854016291582,
-0.656514046006911,-0.439871468993734,-0.223283558174501,0.),
 .UNSPECIFIED.);
#1236=B_SPLINE_CURVE_WITH_KNOTS('',3,(#33139,#33140,#33141,#33142,#33143,
#33144),.UNSPECIFIED.,.F.,.F.,(4,2,4),(-0.236447869261725,-0.118223934265819,
0.),.UNSPECIFIED.);
#1237=B_SPLINE_CURVE_WITH_KNOTS('',3,(#33155,#33156,#33157,#33158,#33159,
#33160),.UNSPECIFIED.,.F.,.F.,(4,2,4),(0.,0.147316860903661,0.298566671239079),
 .UNSPECIFIED.);
#1238=B_SPLINE_CURVE_WITH_KNOTS('',3,(#33161,#33162,#33163,#33164,#33165,
#33166),.UNSPECIFIED.,.F.,.F.,(4,2,4),(0.,0.155861462063028,0.306744458244242),
 .UNSPECIFIED.);
#1239=B_SPLINE_CURVE_WITH_KNOTS('',3,(#33177,#33178,#33179,#33180,#33181,
#33182,#33183,#33184,#33185,#33186),.UNSPECIFIED.,.F.,.F.,(4,2,2,2,4),(0.,
0.212413059834235,0.422510962127527,0.653050142710767,0.893897606534324),
 .UNSPECIFIED.);
#1240=B_SPLINE_CURVE_WITH_KNOTS('',3,(#33191,#33192,#33193,#33194,#33195,
#33196),.UNSPECIFIED.,.F.,.F.,(4,2,4),(-0.21923729130139,-0.109655629737214,
0.),.UNSPECIFIED.);
#1241=B_SPLINE_CURVE_WITH_KNOTS('',3,(#33206,#33207,#33208,#33209,#33210,
#33211,#33212,#33213),.UNSPECIFIED.,.F.,.F.,(4,2,2,4),(1.00620996162504E-6,
0.71712566206726,1.45409684772959,2.51788337929663),.UNSPECIFIED.);
#1242=B_SPLINE_CURVE_WITH_KNOTS('',3,(#33214,#33215,#33216,#33217,#33218,
#33219),.UNSPECIFIED.,.F.,.F.,(4,2,4),(0.,0.273557576637765,0.489035686879138),
 .UNSPECIFIED.);
#1243=B_SPLINE_CURVE_WITH_KNOTS('',3,(#33220,#33221,#33222,#33223,#33224,
#33225),.UNSPECIFIED.,.F.,.F.,(4,2,4),(0.,0.139626851787869,0.274479307755968),
 .UNSPECIFIED.);
#1244=B_SPLINE_CURVE_WITH_KNOTS('',3,(#33242,#33243,#33244,#33245,#33246,
#33247),.UNSPECIFIED.,.F.,.F.,(4,2,4),(-1.31305950518371,-0.674802781976278,
0.),.UNSPECIFIED.);
#1245=B_SPLINE_CURVE_WITH_KNOTS('',3,(#33296,#33297,#33298,#33299,#33300,
#33301,#33302,#33303,#33304,#33305,#33306,#33307,#33308,#33309,#33310,#33311,
#33312,#33313,#33314,#33315,#33316,#33317),.UNSPECIFIED.,.F.,.F.,(4,2,2,
2,2,2,2,2,2,2,4),(-0.67702556757787,-0.651718544287976,-0.630843443379476,
-0.58908983016846,-0.505569216727294,-0.338477588334701,-0.171470508905719,
-0.087950579362434,-0.04618670809926,-0.0253037910690105,-9.99986766170302E-7),
 .UNSPECIFIED.);
#1246=B_SPLINE_CURVE_WITH_KNOTS('',3,(#33327,#33328,#33329,#33330,#33331,
#33332),.UNSPECIFIED.,.F.,.F.,(4,2,4),(-0.20312688170718,-0.101605684816453,
0.),.UNSPECIFIED.);
#1247=B_SPLINE_CURVE_WITH_KNOTS('',3,(#33361,#33362,#33363,#33364,#33365,
#33366),.UNSPECIFIED.,.F.,.F.,(4,2,4),(1.00620234016808E-6,0.51961835527925,
1.02113839753968),.UNSPECIFIED.);
#1248=B_SPLINE_CURVE_WITH_KNOTS('',3,(#33367,#33368,#33369,#33370,#33371,
#33372),.UNSPECIFIED.,.F.,.F.,(4,2,4),(1.15442842194411,1.861681583331,
2.51727485684938),.UNSPECIFIED.);
#1249=B_SPLINE_CURVE_WITH_KNOTS('',3,(#33417,#33418,#33419,#33420,#33421,
#33422),.UNSPECIFIED.,.F.,.F.,(4,2,4),(-0.219070150136512,-0.109422426323688,
0.),.UNSPECIFIED.);
#1250=B_SPLINE_CURVE_WITH_KNOTS('',3,(#33442,#33443,#33444,#33445,#33446,
#33447),.UNSPECIFIED.,.F.,.F.,(4,2,4),(-0.219070150454542,-0.10976760949543,
0.),.UNSPECIFIED.);
#1251=B_SPLINE_CURVE_WITH_KNOTS('',3,(#33502,#33503,#33504,#33505,#33506,
#33507,#33508,#33509,#33510,#33511,#33512,#33513,#33514,#33515,#33516,#33517,
#33518,#33519,#33520,#33521,#33522,#33523,#33524,#33525),.UNSPECIFIED.,
 .F.,.F.,(4,2,2,2,2,2,2,2,2,2,2,4),(-0.689781963483316,-0.663919875534272,
-0.64257964545,-0.599900589922741,-0.514548378234951,-0.343871644022324,
-0.173035127373472,-0.0876435221726812,-0.0449550934221477,-0.0236127939716027,
-0.0129421303647674,-9.99973913562435E-7),.UNSPECIFIED.);
#1252=B_SPLINE_CURVE_WITH_KNOTS('',3,(#33534,#33535,#33536,#33537,#33538,
#33539,#33540,#33541),.UNSPECIFIED.,.F.,.F.,(4,2,2,4),(-1.66037250641965,
-0.87290811148185,-0.0419427109352258,0.),.UNSPECIFIED.);
#1253=B_SPLINE_CURVE_WITH_KNOTS('',3,(#33544,#33545,#33546,#33547,#33548,
#33549),.UNSPECIFIED.,.F.,.F.,(4,2,4),(0.,1.22223732175759,2.95853995676252),
 .UNSPECIFIED.);
#1254=B_SPLINE_CURVE_WITH_KNOTS('',3,(#33550,#33551,#33552,#33553),
 .UNSPECIFIED.,.F.,.F.,(4,4),(-23.1972630946761,-22.347414707605),
 .UNSPECIFIED.);
#1255=B_SPLINE_CURVE_WITH_KNOTS('',3,(#33558,#33559,#33560,#33561,#33562,
#33563),.UNSPECIFIED.,.F.,.F.,(4,2,4),(9.99999994860392E-7,0.112313919124985,
0.224652231943206),.UNSPECIFIED.);
#1256=B_SPLINE_CURVE_WITH_KNOTS('',3,(#33628,#33629,#33630,#33631,#33632,
#33633),.UNSPECIFIED.,.F.,.F.,(4,2,4),(0.,0.20854145283333,0.373296784857941),
 .UNSPECIFIED.);
#1257=B_SPLINE_CURVE_WITH_KNOTS('',3,(#33636,#33637,#33638,#33639,#33640,
#33641),.UNSPECIFIED.,.F.,.F.,(4,2,4),(9.99999986949769E-7,0.158932365867243,
0.391091294154302),.UNSPECIFIED.);
#1258=B_SPLINE_CURVE_WITH_KNOTS('',3,(#33708,#33709,#33710,#33711,#33712,
#33713),.UNSPECIFIED.,.F.,.F.,(4,2,4),(1.03330465267236E-6,0.182634881882751,
0.383588358675),.UNSPECIFIED.);
#1259=B_SPLINE_CURVE_WITH_KNOTS('',3,(#33718,#33719,#33720,#33721,#33722,
#33723),.UNSPECIFIED.,.F.,.F.,(4,2,4),(9.999997436785E-7,0.113920800023667,
0.228887545318261),.UNSPECIFIED.);
#1260=B_SPLINE_CURVE_WITH_KNOTS('',3,(#33790,#33791,#33792,#33793,#33794,
#33795),.UNSPECIFIED.,.F.,.F.,(4,2,4),(9.99999083278551E-7,0.12313457024449,
0.288846007336836),.UNSPECIFIED.);
#1261=B_SPLINE_CURVE_WITH_KNOTS('',3,(#33796,#33797,#33798,#33799,#33800,
#33801),.UNSPECIFIED.,.F.,.F.,(4,2,4),(9.99991096902383E-7,0.078379741412785,
0.129432320943639),.UNSPECIFIED.);
#1262=B_SPLINE_CURVE_WITH_KNOTS('',3,(#33868,#33869,#33870,#33871,#33872,
#33873),.UNSPECIFIED.,.F.,.F.,(4,2,4),(9.99989423159434E-7,0.211833339665523,
0.42360307281474),.UNSPECIFIED.);
#1263=B_SPLINE_CURVE_WITH_KNOTS('',3,(#33878,#33879,#33880,#33881,#33882,
#33883),.UNSPECIFIED.,.F.,.F.,(4,2,4),(9.99999996036891E-7,0.11189630300938,
0.221776909200746),.UNSPECIFIED.);
#1264=B_SPLINE_CURVE_WITH_KNOTS('',3,(#33950,#33951,#33952,#33953,#33954,
#33955),.UNSPECIFIED.,.F.,.F.,(4,2,4),(1.00000031278451E-6,0.146046673780185,
0.369899176224888),.UNSPECIFIED.);
#1265=B_SPLINE_CURVE_WITH_KNOTS('',3,(#33956,#33957,#33958,#33959,#33960,
#33961),.UNSPECIFIED.,.F.,.F.,(4,2,4),(9.99963678285791E-7,0.0529579303912984,
0.0924045001196666),.UNSPECIFIED.);
#1266=B_SPLINE_CURVE_WITH_KNOTS('',3,(#34028,#34029,#34030,#34031,#34032,
#34033),.UNSPECIFIED.,.F.,.F.,(4,2,4),(9.99986781446215E-7,0.170524601610324,
0.324175091837708),.UNSPECIFIED.);
#1267=B_SPLINE_CURVE_WITH_KNOTS('',3,(#34038,#34039,#34040,#34041,#34042,
#34043),.UNSPECIFIED.,.F.,.F.,(4,2,4),(1.0000000011459E-6,0.112462083036288,
0.225270672274139),.UNSPECIFIED.);
#1268=B_SPLINE_CURVE_WITH_KNOTS('',3,(#34109,#34110,#34111,#34112,#34113,
#34114),.UNSPECIFIED.,.F.,.F.,(4,2,4),(9.99378738311195E-7,1.48487197654131,
3.23722575134267),.UNSPECIFIED.);
#1269=B_SPLINE_CURVE_WITH_KNOTS('',3,(#34115,#34116,#34117,#34118,#34119,
#34120),.UNSPECIFIED.,.F.,.F.,(4,2,4),(9.99999984664222E-7,0.280996171754984,
0.634468298631835),.UNSPECIFIED.);
#1270=B_SPLINE_CURVE_WITH_KNOTS('',3,(#34121,#34122,#34123,#34124,#34125,
#34126),.UNSPECIFIED.,.F.,.F.,(4,2,4),(9.9997018998747E-7,0.0631262577557768,
0.106314027062238),.UNSPECIFIED.);
#1271=B_SPLINE_CURVE_WITH_KNOTS('',3,(#34168,#34169,#34170,#34171,#34172,
#34173,#34174,#34175,#34176,#34177,#34178,#34179,#34180,#34181,#34182,#34183,
#34184,#34185,#34186,#34187,#34188,#34189,#34190,#34191,#34192,#34193,#34194,
#34195,#34196,#34197,#34198,#34199,#34200,#34201,#34202,#34203,#34204,#34205,
#34206,#34207,#34208,#34209,#34210,#34211,#34212,#34213,#34214,#34215,#34216,
#34217,#34218,#34219,#34220,#34221,#34222,#34223,#34224,#34225,#34226,#34227,
#34228,#34229,#34230,#34231,#34232,#34233,#34234,#34235,#34236,#34237,#34238,
#34239,#34240,#34241,#34242,#34243,#34244,#34245,#34246,#34247,#34248,#34249,
#34250,#34251,#34252,#34253,#34254,#34255),.UNSPECIFIED.,.F.,.F.,(4,3,3,
3,3,3,3,3,3,3,3,3,3,3,3,3,3,3,3,3,3,3,3,3,3,3,3,3,3,4),(0.,0.166675928619695,
0.173691671300186,0.254448942023543,0.294348326144002,0.333295697963079,
0.383467607004402,0.499995091497343,0.500000000000883,0.570172751020376,
0.666571417474997,0.666664431569024,0.670314863554253,0.674854874036545,
0.749023437501325,0.750000000001324,0.812500000001118,0.836217353799779,
0.836971115969276,0.837080348477548,0.837120435215152,0.843750000001017,
0.867187500000943,0.874511718750916,0.875000000000913,0.906458280152192,
0.943531800863156,0.995806241052779,0.999114427440319,1.),.UNSPECIFIED.);
#1272=B_SPLINE_CURVE_WITH_KNOTS('',3,(#34256,#34257,#34258,#34259,#34260,
#34261,#34262),.UNSPECIFIED.,.F.,.F.,(4,3,4),(8.05019156257696E-11,0.00536781103725429,
0.00861833511932773),.UNSPECIFIED.);
#1273=B_SPLINE_CURVE_WITH_KNOTS('',3,(#35884,#35885,#35886,#35887,#35888,
#35889,#35890,#35891,#35892,#35893,#35894,#35895,#35896,#35897,#35898,#35899,
#35900,#35901,#35902,#35903,#35904,#35905,#35906,#35907,#35908,#35909,#35910,
#35911,#35912,#35913,#35914,#35915,#35916,#35917,#35918,#35919,#35920,#35921,
#35922,#35923,#35924,#35925,#35926,#35927),.UNSPECIFIED.,.F.,.F.,(4,2,1,
1,1,1,2,2,2,1,1,1,2,2,2,2,2,1,2,2,2,1,1,1,1,2,2,4),(0.,0.249999999994906,
0.374999999992358,0.437499999991084,0.468749999990448,0.484374999990131,
0.499755859364856,0.499999999989862,0.562499999991161,0.59374999999181,
0.609374999992134,0.617187499992296,0.623046874992423,0.624999999992465,
0.687499999993976,0.695312499994169,0.703124999994362,0.718749999994754,
0.749023437495509,0.74999999999553,0.812499999996658,0.843749999997218,
0.859374999997502,0.867187499997643,0.871093749997717,0.874023437497773,
0.874999999997791,1.),.UNSPECIFIED.);
#1274=B_SPLINE_CURVE_WITH_KNOTS('',3,(#35928,#35929,#35930,#35931,#35932,
#35933,#35934,#35935,#35936,#35937,#35938,#35939,#35940,#35941,#35942,#35943,
#35944,#35945,#35946,#35947,#35948,#35949,#35950,#35951),.UNSPECIFIED.,
 .F.,.F.,(4,2,2,2,2,2,2,2,2,2,2,4),(1.01547833161899E-13,0.15566333494698,
0.311333269417955,0.622613162774609,0.829990346854508,1.24450593125942,
1.45160761783459,1.55514057778074,1.60689756195558,1.63277301939669,1.6457099117961,
1.66147743182145),.UNSPECIFIED.);
#1275=B_SPLINE_CURVE_WITH_KNOTS('',3,(#35968,#35969,#35970,#35971,#35972,
#35973,#35974,#35975,#35976,#35977),.UNSPECIFIED.,.F.,.F.,(4,3,3,4),(0.,
0.00439626310689482,0.00879197415188345,0.0108268048064541),
 .UNSPECIFIED.);
#1276=B_SPLINE_CURVE_WITH_KNOTS('',3,(#35992,#35993,#35994,#35995,#35996,
#35997),.UNSPECIFIED.,.F.,.F.,(4,2,4),(-0.203125620789724,-0.101587706586047,
0.),.UNSPECIFIED.);
#1277=B_SPLINE_CURVE_WITH_KNOTS('',3,(#36015,#36016,#36017,#36018),
 .UNSPECIFIED.,.F.,.F.,(4,4),(6.93889390390723E-18,0.0131542251006493),
 .UNSPECIFIED.);
#1278=B_SPLINE_CURVE_WITH_KNOTS('',3,(#36019,#36020,#36021,#36022,#36023,
#36024,#36025,#36026),.UNSPECIFIED.,.F.,.F.,(4,2,2,4),(1.00147320738661E-6,
0.717114068453892,1.45422582770195,2.51726157849465),.UNSPECIFIED.);
#1279=B_SPLINE_CURVE_WITH_KNOTS('',3,(#36044,#36045,#36046,#36047,#36048,
#36049,#36050,#36051),.UNSPECIFIED.,.F.,.F.,(4,2,2,4),(9.99999983042343E-7,
1.05770788847698,1.79140562198516,2.50518852593767),.UNSPECIFIED.);
#1280=B_SPLINE_CURVE_WITH_KNOTS('',3,(#36052,#36053,#36054,#36055,#36056,
#36057),.UNSPECIFIED.,.F.,.F.,(4,2,4),(-1.31507690872101,-0.657539408413606,
-9.8734492248731E-7),.UNSPECIFIED.);
#1281=B_SPLINE_CURVE_WITH_KNOTS('',3,(#36071,#36072,#36073,#36074,#36075,
#36076),.UNSPECIFIED.,.F.,.F.,(4,2,4),(1.00970492822167E-6,0.246544274330857,
0.495341408835484),.UNSPECIFIED.);
#1282=B_SPLINE_CURVE_WITH_KNOTS('',3,(#36079,#36080,#36081,#36082,#36083,
#36084),.UNSPECIFIED.,.F.,.F.,(4,2,4),(1.00000002958826E-6,0.141407464738658,
0.282694947289526),.UNSPECIFIED.);
#1283=B_SPLINE_CURVE_WITH_KNOTS('',3,(#36095,#36096,#36097,#36098,#36099,
#36100,#36101,#36102,#36103,#36104),.UNSPECIFIED.,.F.,.F.,(4,2,2,2,4),(0.,
0.227646793319022,0.445793915542063,0.66886948512083,0.894190037790346),
 .UNSPECIFIED.);
#1284=B_SPLINE_CURVE_WITH_KNOTS('',3,(#36109,#36110,#36111,#36112,#36113,
#36114),.UNSPECIFIED.,.F.,.F.,(4,2,4),(-0.219067405041613,-0.109420963077563,
0.),.UNSPECIFIED.);
#1285=B_SPLINE_CURVE_WITH_KNOTS('',3,(#36125,#36126,#36127,#36128,#36129,
#36130),.UNSPECIFIED.,.F.,.F.,(4,2,4),(0.,0.157819485234147,0.315476292188043),
 .UNSPECIFIED.);
#1286=B_SPLINE_CURVE_WITH_KNOTS('',3,(#36131,#36132,#36133,#36134,#36135,
#36136),.UNSPECIFIED.,.F.,.F.,(4,2,4),(0.,0.153590633707747,0.307315056675274),
 .UNSPECIFIED.);
#1287=B_SPLINE_CURVE_WITH_KNOTS('',3,(#36147,#36148,#36149,#36150,#36151,
#36152,#36153,#36154,#36155,#36156),.UNSPECIFIED.,.F.,.F.,(4,2,2,2,4),(0.,
0.223290793074201,0.43983513202536,0.656542865977632,0.880002105353678),
 .UNSPECIFIED.);
#1288=B_SPLINE_CURVE_WITH_KNOTS('',3,(#36161,#36162,#36163,#36164,#36165,
#36166),.UNSPECIFIED.,.F.,.F.,(4,2,4),(-0.219067432347822,-0.109533716096716,
0.),.UNSPECIFIED.);
#1289=B_SPLINE_CURVE_WITH_KNOTS('',3,(#36177,#36178,#36179,#36180,#36181,
#36182),.UNSPECIFIED.,.F.,.F.,(4,2,4),(0.,0.153696799307367,0.30725981325678),
 .UNSPECIFIED.);
#1290=B_SPLINE_CURVE_WITH_KNOTS('',3,(#36183,#36184,#36185,#36186,#36187,
#36188),.UNSPECIFIED.,.F.,.F.,(4,2,4),(0.,0.157693074719598,0.315548927891733),
 .UNSPECIFIED.);
#1291=B_SPLINE_CURVE_WITH_KNOTS('',3,(#36199,#36200,#36201,#36202,#36203,
#36204,#36205,#36206,#36207,#36208),.UNSPECIFIED.,.F.,.F.,(4,2,2,2,4),(0.,
0.225387094225478,0.448531943602552,0.66660741501709,0.894174761832726),
 .UNSPECIFIED.);
#1292=B_SPLINE_CURVE_WITH_KNOTS('',3,(#36217,#36218,#36219,#36220,#36221,
#36222),.UNSPECIFIED.,.F.,.F.,(4,2,4),(1.44977320229459E-15,0.24697660625387,
0.494938254641676),.UNSPECIFIED.);
#1293=B_SPLINE_CURVE_WITH_KNOTS('',3,(#36223,#36224,#36225,#36226,#36227,
#36228),.UNSPECIFIED.,.F.,.F.,(4,2,4),(0.,0.141299010574654,0.282729372489341),
 .UNSPECIFIED.);
#1294=B_SPLINE_CURVE_WITH_KNOTS('',3,(#36285,#36286,#36287,#36288),
 .UNSPECIFIED.,.F.,.F.,(4,4),(4.11130213194751E-6,0.999911030802199),
 .UNSPECIFIED.);
#1295=B_SPLINE_CURVE_WITH_KNOTS('',3,(#36321,#36322,#36323,#36324,#36325,
#36326),.UNSPECIFIED.,.F.,.F.,(4,2,4),(-0.291319261775491,-0.159787359154877,
0.),.UNSPECIFIED.);
#1296=B_SPLINE_CURVE_WITH_KNOTS('',3,(#36329,#36330,#36331,#36332,#36333,
#36334),.UNSPECIFIED.,.F.,.F.,(4,2,4),(-0.942062317972325,-0.782274958817505,
-0.650743056196821),.UNSPECIFIED.);
#1297=B_SPLINE_CURVE_WITH_KNOTS('',3,(#36343,#36344,#36345,#36346,#36347,
#36348),.UNSPECIFIED.,.F.,.F.,(4,2,4),(-0.29131926177555,-0.159787359154858,
-3.46389583683049E-14),.UNSPECIFIED.);
#1298=B_SPLINE_CURVE_WITH_KNOTS('',3,(#36351,#36352,#36353,#36354,#36355,
#36356),.UNSPECIFIED.,.F.,.F.,(4,2,4),(-0.94206231797227,-0.782274958817496,
-0.650743056196749),.UNSPECIFIED.);
#1299=B_SPLINE_CURVE_WITH_KNOTS('',3,(#36359,#36360,#36361,#36362,#36363,
#36364),.UNSPECIFIED.,.F.,.F.,(4,2,4),(-0.299277276892238,-0.149638638446119,
0.),.UNSPECIFIED.);
#1300=B_SPLINE_CURVE_WITH_KNOTS('',3,(#36368,#36369,#36370,#36371,#36372,
#36373),.UNSPECIFIED.,.F.,.F.,(4,2,4),(-0.942062317972285,-0.782274958817465,
-0.650743056196774),.UNSPECIFIED.);
#1301=B_SPLINE_CURVE_WITH_KNOTS('',3,(#36379,#36380,#36381,#36382,#36383,
#36384),.UNSPECIFIED.,.F.,.F.,(4,2,4),(-0.291319261775506,-0.15978735915482,
0.),.UNSPECIFIED.);
#1302=B_SPLINE_CURVE_WITH_KNOTS('',3,(#36387,#36388,#36389,#36390,#36391,
#36392),.UNSPECIFIED.,.F.,.F.,(4,2,4),(-0.942062317972366,-0.792423679526272,
-0.642785041080179),.UNSPECIFIED.);
#1303=B_SPLINE_CURVE_WITH_KNOTS('',3,(#36445,#36446,#36447,#36448,#36449,
#36450),.UNSPECIFIED.,.F.,.F.,(4,2,4),(7.05548697529559E-15,0.00523107916144303,
0.010462158322879),.UNSPECIFIED.);
#1304=B_SPLINE_CURVE_WITH_KNOTS('',3,(#36455,#36456,#36457,#36458,#36459,
#36460,#36461,#36462,#36463,#36464,#36465,#36466,#36467,#36468),
 .UNSPECIFIED.,.F.,.F.,(4,2,2,2,2,2,4),(1.00000023840693E-6,0.2965902763434,
0.65268898649409,1.00818635283356,1.36397466372344,1.98488039747023,2.01473577478548),
 .UNSPECIFIED.);
#1305=B_SPLINE_CURVE_WITH_KNOTS('',3,(#36521,#36522,#36523,#36524,#36525,
#36526,#36527,#36528,#36529,#36530,#36531,#36532,#36533,#36534,#36535,#36536,
#36537,#36538,#36539,#36540,#36541,#36542),.UNSPECIFIED.,.F.,.F.,(4,2,2,
2,2,2,2,2,2,2,4),(9.99322294003157E-7,0.011417887542787,0.0222845745097274,
0.0440049682421546,0.0874125886811494,0.174267175958524,0.261121619243541,
0.304529168043487,0.326249525934761,0.337116194970005,0.348534141656),
 .UNSPECIFIED.);
#1306=B_SPLINE_CURVE_WITH_KNOTS('',3,(#36592,#36593,#36594,#36595,#36596,
#36597),.UNSPECIFIED.,.F.,.F.,(4,2,4),(9.13855224931671E-16,0.00523107914708959,
0.0104621582941783),.UNSPECIFIED.);
#1307=B_SPLINE_CURVE_WITH_KNOTS('',3,(#36599,#36600,#36601,#36602,#36603,
#36604,#36605,#36606,#36607,#36608,#36609,#36610,#36611,#36612),
 .UNSPECIFIED.,.F.,.F.,(4,2,2,2,2,2,4),(9.99999960801238E-7,0.0410400374680066,
0.66754883484164,1.04225619039533,1.42067016209639,1.80065436420091,2.13788105830901),
 .UNSPECIFIED.);
#1308=B_SPLINE_CURVE_WITH_KNOTS('',3,(#36668,#36669,#36670,#36671,#36672,
#36673,#36674,#36675,#36676,#36677,#36678,#36679,#36680,#36681),
 .UNSPECIFIED.,.F.,.F.,(4,2,2,2,2,2,4),(-1.99242246967209,-1.69912264605073,
-1.34696492109298,-0.995397472045463,-0.643553467950021,-0.0295448893533265,
-9.99999972400604E-7),.UNSPECIFIED.);
#1309=B_SPLINE_CURVE_WITH_KNOTS('',3,(#36682,#36683,#36684,#36685,#36686,
#36687),.UNSPECIFIED.,.F.,.F.,(4,2,4),(2.97263381041754E-14,0.00523107914593693,
0.0104621582918441),.UNSPECIFIED.);
#1310=B_SPLINE_CURVE_WITH_KNOTS('',3,(#36739,#36740,#36741,#36742,#36743,
#36744,#36745,#36746,#36747,#36748,#36749,#36750,#36751,#36752,#36753,#36754,
#36755,#36756,#36757,#36758,#36759,#36760),.UNSPECIFIED.,.F.,.F.,(4,2,2,
2,2,2,2,2,2,2,4),(-0.34853295910873,-0.337115227653266,-0.32624857232804,
-0.304528241839957,-0.261120747808474,-0.174266413464672,-0.0874122231124873,
-0.0440048007218869,-0.0222845060773082,-0.0114178686877548,-9.99322293774237E-7),
 .UNSPECIFIED.);
#1311=B_SPLINE_CURVE_WITH_KNOTS('',3,(#36811,#36812,#36813,#36814,#36815,
#36816),.UNSPECIFIED.,.F.,.F.,(4,2,4),(1.24917436300588E-15,0.00523107916140929,
0.0104621583229247),.UNSPECIFIED.);
#1312=B_SPLINE_CURVE_WITH_KNOTS('',3,(#36818,#36819,#36820,#36821,#36822,
#36823,#36824,#36825,#36826,#36827,#36828,#36829,#36830,#36831),
 .UNSPECIFIED.,.F.,.F.,(4,2,2,2,2,2,4),(-1.54593699203168,-1.51627628058056,
-1.06322836063848,-0.792267283873332,-0.518634619264518,-0.243863513378528,
-9.99999280715258E-7),.UNSPECIFIED.);
#1313=B_SPLINE_CURVE_WITH_KNOTS('',3,(#36887,#36888,#36889,#36890,#36891,
#36892,#36893,#36894,#36895,#36896,#36897,#36898,#36899,#36900),
 .UNSPECIFIED.,.F.,.F.,(4,2,2,2,2,2,4),(-2.0247534649149,-1.7026576276926,
-1.34880623927078,-0.995849757258031,-0.643258648524814,-0.0288142926510343,
-9.99999972288645E-7),.UNSPECIFIED.);
#1314=B_SPLINE_CURVE_WITH_KNOTS('',3,(#36901,#36902,#36903,#36904,#36905,
#36906,#36907),.UNSPECIFIED.,.F.,.F.,(4,3,4),(1.73056695609661E-14,0.00523109611618601,
0.0104552267462395),.UNSPECIFIED.);
#1315=B_SPLINE_CURVE_WITH_KNOTS('',3,(#36959,#36960,#36961,#36962,#36963,
#36964,#36965,#36966,#36967,#36968,#36969,#36970,#36971,#36972,#36973,#36974,
#36975,#36976,#36977,#36978,#36979,#36980),.UNSPECIFIED.,.F.,.F.,(4,2,2,
2,2,2,2,2,2,2,4),(-0.348530046369699,-0.337112119683411,-0.326245568052259,
-0.304525444827838,-0.261118365012474,-0.174264859478894,-0.0874114979360114,
-0.0440044897577281,-0.0222844023781863,-0.0114178686869934,-9.9932229816912E-7),
 .UNSPECIFIED.);
#1316=B_SPLINE_CURVE_WITH_KNOTS('',3,(#37033,#37034,#37035,#37036,#37037,
#37038,#37039,#37040,#37041,#37042,#37043,#37044,#37045,#37046),
 .UNSPECIFIED.,.F.,.F.,(4,2,2,2,2,2,4),(-1.70662420609644,-1.45502819722534,
-1.20126789349393,-0.996223548128144,-0.767391103085636,-0.365223297458236,
-1.00000010760937E-6),.UNSPECIFIED.);
#1317=B_SPLINE_CURVE_WITH_KNOTS('',3,(#37103,#37104,#37105,#37106,#37107,
#37108,#37109,#37110,#37111,#37112,#37113,#37114,#37115,#37116),
 .UNSPECIFIED.,.F.,.F.,(4,2,2,2,2,2,4),(1.00000005213949E-6,0.373786457125504,
0.781780831542326,1.04178058769923,1.27449283557987,1.5610312787827,1.85194823288523),
 .UNSPECIFIED.);
#1318=B_SPLINE_CURVE_WITH_KNOTS('',3,(#37169,#37170,#37171,#37172,#37173,
#37174,#37175,#37176,#37177,#37178,#37179,#37180,#37181,#37182,#37183,#37184,
#37185,#37186,#37187,#37188,#37189,#37190),.UNSPECIFIED.,.F.,.F.,(4,2,2,
2,2,2,2,2,2,2,4),(9.99322295139288E-7,0.0114188541247426,0.0222854506093803,
0.0440056634961537,0.087412922514029,0.174266786615345,0.26112050672579,
0.30452769410305,0.326247871147981,0.337114449697216,0.348532261911283),
 .UNSPECIFIED.);
#1319=B_SPLINE_CURVE_WITH_KNOTS('',3,(#37240,#37241,#37242,#37243,#37244,
#37245),.UNSPECIFIED.,.F.,.F.,(4,2,4),(4.38854183572088E-17,0.00523107914592229,
0.0104621582918445),.UNSPECIFIED.);
#1320=B_SPLINE_CURVE_WITH_KNOTS('',3,(#37247,#37248,#37249,#37250,#37251,
#37252,#37253,#37254,#37255,#37256,#37257,#37258,#37259,#37260),
 .UNSPECIFIED.,.F.,.F.,(4,2,2,2,2,2,4),(9.99999961583338E-7,0.041041854241271,
0.667547702208066,1.04225347352809,1.42066695540823,1.80065028480642,2.13787646890171),
 .UNSPECIFIED.);
#1321=B_SPLINE_CURVE_WITH_KNOTS('',3,(#37319,#37320,#37321,#37322),
 .UNSPECIFIED.,.F.,.F.,(4,4),(0.,0.0275043317552308),.UNSPECIFIED.);
#1322=B_SPLINE_CURVE_WITH_KNOTS('',3,(#37333,#37334,#37335,#37336),
 .UNSPECIFIED.,.F.,.F.,(4,4),(4.997930709674E-16,0.0275043317552307),
 .UNSPECIFIED.);
#1323=B_SPLINE_CURVE_WITH_KNOTS('',3,(#37349,#37350,#37351,#37352),
 .UNSPECIFIED.,.F.,.F.,(4,4),(4.997930709674E-16,0.0275043317552307),
 .UNSPECIFIED.);
#1324=B_SPLINE_CURVE_WITH_KNOTS('',3,(#37363,#37364,#37365,#37366),
 .UNSPECIFIED.,.F.,.F.,(4,4),(4.997930709674E-16,0.0275043317552318),
 .UNSPECIFIED.);
#1325=B_SPLINE_CURVE_WITH_KNOTS('',3,(#37373,#37374,#37375,#37376),
 .UNSPECIFIED.,.F.,.F.,(4,4),(0.,0.0275043309106357),.UNSPECIFIED.);
#1326=B_SPLINE_CURVE_WITH_KNOTS('',3,(#37387,#37388,#37389,#37390),
 .UNSPECIFIED.,.F.,.F.,(4,4),(0.,0.0275045756311934),.UNSPECIFIED.);
#1327=B_SPLINE_CURVE_WITH_KNOTS('',3,(#37403,#37404,#37405,#37406),
 .UNSPECIFIED.,.F.,.F.,(4,4),(0.,0.0275045756311959),.UNSPECIFIED.);
#1328=B_SPLINE_CURVE_WITH_KNOTS('',3,(#37417,#37418,#37419,#37420),
 .UNSPECIFIED.,.F.,.F.,(4,4),(0.,0.0275043317552308),.UNSPECIFIED.);
#1329=B_SPLINE_CURVE_WITH_KNOTS('',3,(#38165,#38166,#38167,#38168,#38169,
#38170,#38171,#38172,#38173,#38174),.UNSPECIFIED.,.F.,.F.,(4,2,2,2,4),(-5.2918916828979,
-5.03351157658279,-4.84005150769012,-4.64659143879744,-4.34027267238539),
 .UNSPECIFIED.);
#1330=B_SPLINE_CURVE_WITH_KNOTS('',3,(#38336,#38337,#38338,#38339,#38340,
#38341),.UNSPECIFIED.,.F.,.F.,(4,2,4),(-0.371374848070398,-0.285575684483783,
-0.218017291375941),.UNSPECIFIED.);
#1331=B_SPLINE_CURVE_WITH_KNOTS('',3,(#38351,#38352,#38353,#38354,#38355,
#38356),.UNSPECIFIED.,.F.,.F.,(4,2,4),(-1.50046812968576,-1.43290973657793,
-1.34711057299131),.UNSPECIFIED.);
#1332=B_SPLINE_CURVE_WITH_KNOTS('',3,(#38550,#38551,#38552,#38553,#38554,
#38555),.UNSPECIFIED.,.F.,.F.,(4,2,4),(-0.524597258187126,-0.399172888862268,
0.),.UNSPECIFIED.);
#1333=B_SPLINE_CURVE_WITH_KNOTS('',3,(#38556,#38557,#38558,#38559,#38560,
#38561),.UNSPECIFIED.,.F.,.F.,(4,2,4),(-4.54956787028548,-4.15039498142321,
-4.02497061209835),.UNSPECIFIED.);
#1334=B_SPLINE_CURVE_WITH_KNOTS('',3,(#38564,#38565,#38566,#38567,#38568,
#38569),.UNSPECIFIED.,.F.,.F.,(4,2,4),(-4.54956787028547,-4.15039498142321,
-4.02497061209835),.UNSPECIFIED.);
#1335=B_SPLINE_CURVE_WITH_KNOTS('',3,(#38570,#38571,#38572,#38573,#38574,
#38575),.UNSPECIFIED.,.F.,.F.,(4,2,4),(-0.524597258187133,-0.399172888862267,
-1.88737914186277E-15),.UNSPECIFIED.);
#1336=B_SPLINE_CURVE_WITH_KNOTS('',3,(#38577,#38578,#38579,#38580,#38581,
#38582),.UNSPECIFIED.,.F.,.F.,(4,2,4),(-4.54910652185684,-4.14993363299457,
-4.02450926366971),.UNSPECIFIED.);
#1337=B_SPLINE_CURVE_WITH_KNOTS('',3,(#38583,#38584,#38585,#38586,#38587,
#38588),.UNSPECIFIED.,.F.,.F.,(4,2,4),(-0.524597258187127,-0.399172888862266,
0.),.UNSPECIFIED.);
#1338=B_SPLINE_CURVE_WITH_KNOTS('',3,(#38591,#38592,#38593,#38594,#38595,
#38596),.UNSPECIFIED.,.F.,.F.,(4,2,4),(-4.54910652185684,-4.14993363299457,
-4.0245092636697),.UNSPECIFIED.);
#1339=B_SPLINE_CURVE_WITH_KNOTS('',3,(#38597,#38598,#38599,#38600),
 .UNSPECIFIED.,.F.,.F.,(4,4),(-0.370064844470512,0.),.UNSPECIFIED.);
#1340=B_SPLINE_CURVE_WITH_KNOTS('',3,(#38604,#38605,#38606,#38607),
 .UNSPECIFIED.,.F.,.F.,(4,4),(-4.54956787028547,-4.17950302581496),
 .UNSPECIFIED.);
#1341=B_SPLINE_CURVE_WITH_KNOTS('',3,(#38608,#38609,#38610,#38611,#38612,
#38613),.UNSPECIFIED.,.F.,.F.,(4,2,4),(-0.524597258187134,-0.399172888862265,
0.),.UNSPECIFIED.);
#1342=B_SPLINE_CURVE_WITH_KNOTS('',3,(#38623,#38624,#38625,#38626,#38627,
#38628),.UNSPECIFIED.,.F.,.F.,(4,2,4),(-0.371374848070411,-0.285575684483777,
-0.218017291375943),.UNSPECIFIED.);
#1343=B_SPLINE_CURVE_WITH_KNOTS('',3,(#38638,#38639,#38640,#38641,#38642,
#38643),.UNSPECIFIED.,.F.,.F.,(4,2,4),(-1.50046812968577,-1.43290973657793,
-1.3471105729913),.UNSPECIFIED.);
#1344=B_SPLINE_CURVE_WITH_KNOTS('',3,(#38648,#38649,#38650,#38651,#38652,
#38653),.UNSPECIFIED.,.F.,.F.,(4,2,4),(-4.54956787028547,-4.15039498142321,
-4.02497061209834),.UNSPECIFIED.);
#1345=B_SPLINE_CURVE_WITH_KNOTS('',3,(#38654,#38655,#38656,#38657,#38658,
#38659),.UNSPECIFIED.,.F.,.F.,(4,2,4),(-0.524597258187132,-0.399172888862266,
0.),.UNSPECIFIED.);
#1346=B_SPLINE_CURVE_WITH_KNOTS('',3,(#38661,#38662,#38663,#38664,#38665,
#38666),.UNSPECIFIED.,.F.,.F.,(4,2,4),(-4.54910652185684,-4.14993363299457,
-4.02450926366973),.UNSPECIFIED.);
#1347=B_SPLINE_CURVE_WITH_KNOTS('',3,(#38667,#38668,#38669,#38670,#38671,
#38672),.UNSPECIFIED.,.F.,.F.,(4,2,4),(-0.524597258187128,-0.399172888862267,
0.),.UNSPECIFIED.);
#1348=B_SPLINE_CURVE_WITH_KNOTS('',3,(#38675,#38676,#38677,#38678,#38679,
#38680),.UNSPECIFIED.,.F.,.F.,(4,2,4),(-4.54956787028547,-4.15039498142321,
-4.02497061209834),.UNSPECIFIED.);
#1349=B_SPLINE_CURVE_WITH_KNOTS('',3,(#38681,#38682,#38683,#38684,#38685,
#38686),.UNSPECIFIED.,.F.,.F.,(4,2,4),(-0.524597258187134,-0.399172888862263,
0.),.UNSPECIFIED.);
#1350=B_SPLINE_CURVE_WITH_KNOTS('',3,(#38688,#38689,#38690,#38691,#38692,
#38693),.UNSPECIFIED.,.F.,.F.,(4,2,4),(-4.54910652185683,-4.14993363299457,
-4.0245092636697),.UNSPECIFIED.);
#1351=B_SPLINE_CURVE_WITH_KNOTS('',3,(#38694,#38695,#38696,#38697,#38698,
#38699),.UNSPECIFIED.,.F.,.F.,(4,2,4),(-0.524597258187127,-0.399172888862264,
0.),.UNSPECIFIED.);
#1352=B_SPLINE_CURVE_WITH_KNOTS('',3,(#38702,#38703,#38704,#38705,#38706,
#38707),.UNSPECIFIED.,.F.,.F.,(4,2,4),(-4.54910652185684,-4.14993363299457,
-4.02450926366971),.UNSPECIFIED.);
#1353=B_SPLINE_CURVE_WITH_KNOTS('',3,(#38710,#38711,#38712,#38713,#38714,
#38715),.UNSPECIFIED.,.F.,.F.,(4,2,4),(-0.52459725818713,-0.399172888862267,
0.),.UNSPECIFIED.);
#1354=B_SPLINE_CURVE_WITH_KNOTS('',3,(#38744,#38745,#38746,#38747,#38748,
#38749,#38750,#38751,#38752,#38753,#38754,#38755,#38756,#38757,#38758,#38759,
#38760,#38761,#38762,#38763,#38764,#38765,#38766,#38767,#38768,#38769,#38770,
#38771,#38772,#38773,#38774,#38775,#38776,#38777,#38778,#38779,#38780,#38781,
#38782,#38783,#38784,#38785,#38786),.UNSPECIFIED.,.F.,.F.,(4,3,3,3,3,3,
3,3,3,3,3,3,3,3,4),(0.,0.0872544796701012,0.179967974567206,0.275362932442676,
0.370587215980396,0.437499999999772,0.468749999999765,0.484374999999753,
0.49218749999974,0.496093749999741,0.499999999999741,0.638357505841048,
0.781776182157294,0.891012188806263,0.999999999999994),.UNSPECIFIED.);
#1355=B_SPLINE_CURVE_WITH_KNOTS('',3,(#38788,#38789,#38790,#38791,#38792,
#38793,#38794,#38795,#38796,#38797,#38798,#38799,#38800,#38801,#38802,#38803,
#38804,#38805,#38806,#38807,#38808,#38809,#38810,#38811,#38812,#38813,#38814,
#38815,#38816,#38817,#38818,#38819,#38820,#38821,#38822,#38823,#38824,#38825,
#38826,#38827,#38828,#38829,#38830,#38831,#38832,#38833,#38834,#38835,#38836),
 .UNSPECIFIED.,.F.,.F.,(4,3,3,3,3,3,3,3,3,3,3,3,3,3,3,3,4),(0.,0.09989275696205,
0.197149256723823,0.250000000001032,0.343701993891013,0.443601545051249,
0.497279897256218,0.498046875002055,0.500000000002058,0.571177947453751,
0.641445155754051,0.70984637527501,0.750000000001029,0.813786943013992,
0.876119581926588,0.938059790963294,1.),.UNSPECIFIED.);
#1356=B_SPLINE_CURVE_WITH_KNOTS('',3,(#38837,#38838,#38839,#38840,#38841,
#38842),.UNSPECIFIED.,.F.,.F.,(4,2,4),(-0.241266937338003,-0.121297446584125,
0.),.UNSPECIFIED.);
#1357=B_SPLINE_CURVE_WITH_KNOTS('',3,(#38923,#38924,#38925,#38926,#38927,
#38928),.UNSPECIFIED.,.F.,.F.,(4,2,4),(-0.241267240141802,-0.121297491113608,
0.),.UNSPECIFIED.);
#1358=B_SPLINE_CURVE_WITH_KNOTS('',3,(#38929,#38930,#38931,#38932,#38933,
#38934,#38935,#38936,#38937,#38938,#38939,#38940,#38941,#38942,#38943,#38944,
#38945,#38946,#38947,#38948,#38949,#38950,#38951,#38952,#38953,#38954,#38955,
#38956,#38957,#38958,#38959,#38960,#38961,#38962,#38963,#38964,#38965,#38966,
#38967,#38968,#38969,#38970,#38971,#38972,#38973,#38974,#38975,#38976,#38977),
 .UNSPECIFIED.,.F.,.F.,(4,3,3,3,3,3,3,3,3,3,3,3,3,3,3,3,4),(0.,0.0590959733778193,
0.12064791084943,0.183845110418003,0.245892786158591,0.299888306122572,
0.371749913788964,0.443192297459707,0.498046874999004,0.499999999999002,
0.502720163109487,0.593864795540943,0.686682262709001,0.782202229346505,
0.879448387345353,0.979332662309031,1.),.UNSPECIFIED.);
#1359=B_SPLINE_CURVE_WITH_KNOTS('',3,(#39175,#39176,#39177,#39178,#39179,
#39180),.UNSPECIFIED.,.F.,.F.,(4,2,4),(-0.241267240141382,-0.121297491113753,
0.),.UNSPECIFIED.);
#1360=B_SPLINE_CURVE_WITH_KNOTS('',3,(#39182,#39183,#39184,#39185,#39186,
#39187,#39188,#39189,#39190,#39191,#39192,#39193,#39194,#39195,#39196,#39197,
#39198,#39199,#39200,#39201,#39202,#39203,#39204,#39205,#39206,#39207,#39208,
#39209,#39210,#39211,#39212,#39213,#39214,#39215,#39216,#39217,#39218,#39219,
#39220,#39221,#39222,#39223,#39224,#39225,#39226,#39227,#39228,#39229,#39230),
 .UNSPECIFIED.,.F.,.F.,(4,3,3,3,3,3,3,3,3,3,3,3,3,3,3,3,4),(0.,0.0590959737305276,
0.120647911557508,0.183845111495701,0.245892787653034,0.299888306754146,
0.371749914989915,0.443192319371491,0.498046874999129,0.499999999999131,
0.502720163116374,0.593864796197773,0.686682264014154,0.78220223130903,
0.879448389968442,0.979332665575473,1.),.UNSPECIFIED.);
#1361=B_SPLINE_CURVE_WITH_KNOTS('',3,(#39262,#39263,#39264,#39265,#39266,
#39267,#39268,#39269,#39270,#39271,#39272,#39273,#39274,#39275,#39276,#39277,
#39278,#39279,#39280,#39281,#39282,#39283,#39284,#39285,#39286,#39287,#39288,
#39289,#39290,#39291,#39292,#39293,#39294,#39295,#39296,#39297,#39298,#39299,
#39300,#39301,#39302,#39303,#39304,#39305,#39306,#39307,#39308,#39309,#39310),
 .UNSPECIFIED.,.F.,.F.,(4,3,3,3,3,3,3,3,3,3,3,3,3,3,3,3,4),(0.,0.0998927578409832,
0.197149258553956,0.249999999999427,0.343701994843245,0.443601545265527,
0.497279897243239,0.498046874998851,0.499999999998844,0.571177948292924,
0.64144515738966,0.709846377640365,0.749999999999422,0.813786943534484,
0.876119582949847,0.938059791474924,1.),.UNSPECIFIED.);
#1362=B_SPLINE_CURVE_WITH_KNOTS('',3,(#39311,#39312,#39313,#39314,#39315,
#39316),.UNSPECIFIED.,.F.,.F.,(4,2,4),(-0.24126693733769,-0.121297446583894,
0.),.UNSPECIFIED.);
#1363=B_SPLINE_CURVE_WITH_KNOTS('',3,(#39456,#39457,#39458,#39459,#39460,
#39461,#39462,#39463),.UNSPECIFIED.,.F.,.F.,(4,2,2,4),(1.0455577725842,
1.95553903235196,3.95431621571259,4.41434897542879),.UNSPECIFIED.);
#1364=B_SPLINE_CURVE_WITH_KNOTS('',3,(#39475,#39476,#39477,#39478,#39479,
#39480,#39481,#39482),.UNSPECIFIED.,.F.,.F.,(4,2,2,4),(2.03056498878569,
2.99956672815959,4.49935009223939,4.8962823044381),.UNSPECIFIED.);
#1365=B_SPLINE_CURVE_WITH_KNOTS('',3,(#39636,#39637,#39638,#39639),
 .UNSPECIFIED.,.F.,.F.,(4,4),(-4.87675282368594,-1.08452914514666),
 .UNSPECIFIED.);
#1366=B_SPLINE_CURVE_WITH_KNOTS('',3,(#39644,#39645,#39646,#39647),
 .UNSPECIFIED.,.F.,.F.,(4,4),(-4.87667483628068,-1.08444993827179),
 .UNSPECIFIED.);
#1367=B_SPLINE_CURVE_WITH_KNOTS('',3,(#39650,#39651,#39652,#39653),
 .UNSPECIFIED.,.F.,.F.,(4,4),(-4.87674823462075,-1.08452453146112),
 .UNSPECIFIED.);
#1368=ELLIPSE('',#18362,36.6292398804354,35.);
#1369=ELLIPSE('',#18364,36.6292398804354,35.);
#1370=ELLIPSE('',#18366,36.6292398804354,35.);
#1371=ELLIPSE('',#18368,36.6292398804354,35.);
#1372=ELLIPSE('',#18372,36.6292398804354,35.);
#1373=ELLIPSE('',#18374,36.6292398804354,35.);
#1374=ELLIPSE('',#18376,36.6292398804354,35.);
#1375=ELLIPSE('',#18378,36.6292398804354,35.);
#1376=ELLIPSE('',#18380,36.6292398804354,35.);
#1377=ELLIPSE('',#18924,7.07832284981318,6.99999999999854);
#1378=ELLIPSE('',#18926,7.07832284981318,6.99999999999854);
#1379=ELLIPSE('',#18948,7.0629889670351,6.99999999995947);
#1380=ELLIPSE('',#18952,7.06298896705052,6.9999999999871);
#1381=ELLIPSE('',#18962,23.999999999378,11.9999999993886);
#1382=ELLIPSE('',#18963,23.9999999977437,11.9999999977833);
#1383=ELLIPSE('',#18991,23.9999999996724,11.9999999997014);
#1384=ELLIPSE('',#18992,24.0000000005569,12.0000000005208);
#1385=ELLIPSE('',#19004,7.00423907309944,7.00000000002481);
#1386=ELLIPSE('',#19100,22.0866861336612,22.0548621009617);
#1387=ELLIPSE('',#19101,22.0591508859082,21.9667873157955);
#1388=ELLIPSE('',#19102,22.05915088596,21.9667873158956);
#1389=ELLIPSE('',#19103,22.0711672770103,22.010135576304);
#1390=ELLIPSE('',#19104,22.0646581901642,22.0091682784596);
#1391=ELLIPSE('',#19105,22.0748759515261,22.039900950448);
#1392=ELLIPSE('',#19358,62.7132858513459,44.3213853810186);
#1393=ELLIPSE('',#19361,62.713288482779,44.3213890977139);
#1394=ELLIPSE('',#19364,62.7132852238632,44.321384494158);
#1395=ELLIPSE('',#19365,44.5345980614777,31.4244600121006);
#1396=ELLIPSE('',#19367,44.5346010360152,31.424464205272);
#1397=ELLIPSE('',#19369,62.7132944274914,44.3213974951955);
#1398=ELLIPSE('',#19645,4.50272511841123,4.49999999999998);
#1399=ELLIPSE('',#19681,6.92820323083716,6.00000000034999);
#1400=ELLIPSE('',#19688,23.9999999687057,11.9999999731157);
#1401=ELLIPSE('',#19689,6.92820323020547,5.99999999993053);
#1402=ELLIPSE('',#19731,23.9999999658975,11.9999999709002);
#1403=ELLIPSE('',#19733,6.92820323026176,5.99999999998559);
#1404=ELLIPSE('',#19740,6.92820323018877,6.00000000002855);
#1405=ELLIPSE('',#19757,6.08833509735678,4.61528466193146);
#1406=ELLIPSE('',#19807,6.08086351685543,4.60377817015316);
#1407=ELLIPSE('',#19811,6.08735970830141,4.61379430849458);
#1408=LINE('',#24926,#2981);
#1409=LINE('',#24930,#2982);
#1410=LINE('',#24934,#2983);
#1411=LINE('',#24938,#2984);
#1412=LINE('',#24942,#2985);
#1413=LINE('',#24946,#2986);
#1414=LINE('',#24950,#2987);
#1415=LINE('',#24954,#2988);
#1416=LINE('',#24958,#2989);
#1417=LINE('',#24963,#2990);
#1418=LINE('',#24967,#2991);
#1419=LINE('',#24971,#2992);
#1420=LINE('',#24975,#2993);
#1421=LINE('',#24979,#2994);
#1422=LINE('',#24983,#2995);
#1423=LINE('',#24987,#2996);
#1424=LINE('',#24991,#2997);
#1425=LINE('',#24995,#2998);
#1426=LINE('',#24998,#2999);
#1427=LINE('',#25003,#3000);
#1428=LINE('',#25009,#3001);
#1429=LINE('',#25015,#3002);
#1430=LINE('',#25021,#3003);
#1431=LINE('',#25027,#3004);
#1432=LINE('',#25033,#3005);
#1433=LINE('',#25039,#3006);
#1434=LINE('',#25045,#3007);
#1435=LINE('',#25112,#3008);
#1436=LINE('',#25179,#3009);
#1437=LINE('',#25250,#3010);
#1438=LINE('',#25321,#3011);
#1439=LINE('',#25325,#3012);
#1440=LINE('',#25331,#3013);
#1441=LINE('',#25337,#3014);
#1442=LINE('',#25343,#3015);
#1443=LINE('',#25349,#3016);
#1444=LINE('',#25355,#3017);
#1445=LINE('',#25361,#3018);
#1446=LINE('',#25367,#3019);
#1447=LINE('',#25373,#3020);
#1448=LINE('',#25379,#3021);
#1449=LINE('',#25385,#3022);
#1450=LINE('',#25391,#3023);
#1451=LINE('',#25397,#3024);
#1452=LINE('',#25403,#3025);
#1453=LINE('',#25409,#3026);
#1454=LINE('',#25415,#3027);
#1455=LINE('',#25419,#3028);
#1456=LINE('',#25425,#3029);
#1457=LINE('',#25431,#3030);
#1458=LINE('',#25435,#3031);
#1459=LINE('',#25437,#3032);
#1460=LINE('',#25439,#3033);
#1461=LINE('',#25440,#3034);
#1462=LINE('',#25442,#3035);
#1463=LINE('',#25444,#3036);
#1464=LINE('',#25445,#3037);
#1465=LINE('',#25447,#3038);
#1466=LINE('',#25449,#3039);
#1467=LINE('',#25450,#3040);
#1468=LINE('',#25452,#3041);
#1469=LINE('',#25454,#3042);
#1470=LINE('',#25455,#3043);
#1471=LINE('',#25457,#3044);
#1472=LINE('',#25459,#3045);
#1473=LINE('',#25460,#3046);
#1474=LINE('',#25462,#3047);
#1475=LINE('',#25464,#3048);
#1476=LINE('',#25465,#3049);
#1477=LINE('',#25467,#3050);
#1478=LINE('',#25469,#3051);
#1479=LINE('',#25470,#3052);
#1480=LINE('',#25472,#3053);
#1481=LINE('',#25474,#3054);
#1482=LINE('',#25475,#3055);
#1483=LINE('',#25477,#3056);
#1484=LINE('',#25478,#3057);
#1485=LINE('',#25487,#3058);
#1486=LINE('',#25491,#3059);
#1487=LINE('',#25495,#3060);
#1488=LINE('',#25498,#3061);
#1489=LINE('',#25504,#3062);
#1490=LINE('',#25508,#3063);
#1491=LINE('',#25512,#3064);
#1492=LINE('',#25515,#3065);
#1493=LINE('',#25517,#3066);
#1494=LINE('',#25518,#3067);
#1495=LINE('',#25520,#3068);
#1496=LINE('',#25522,#3069);
#1497=LINE('',#25524,#3070);
#1498=LINE('',#25526,#3071);
#1499=LINE('',#25528,#3072);
#1500=LINE('',#25530,#3073);
#1501=LINE('',#25537,#3074);
#1502=LINE('',#25541,#3075);
#1503=LINE('',#25545,#3076);
#1504=LINE('',#25548,#3077);
#1505=LINE('',#25554,#3078);
#1506=LINE('',#25558,#3079);
#1507=LINE('',#25562,#3080);
#1508=LINE('',#25565,#3081);
#1509=LINE('',#25567,#3082);
#1510=LINE('',#25568,#3083);
#1511=LINE('',#25570,#3084);
#1512=LINE('',#25572,#3085);
#1513=LINE('',#25574,#3086);
#1514=LINE('',#25576,#3087);
#1515=LINE('',#25578,#3088);
#1516=LINE('',#25580,#3089);
#1517=LINE('',#25584,#3090);
#1518=LINE('',#25586,#3091);
#1519=LINE('',#25589,#3092);
#1520=LINE('',#25591,#3093);
#1521=LINE('',#25594,#3094);
#1522=LINE('',#25596,#3095);
#1523=LINE('',#25599,#3096);
#1524=LINE('',#25601,#3097);
#1525=LINE('',#25604,#3098);
#1526=LINE('',#25606,#3099);
#1527=LINE('',#25609,#3100);
#1528=LINE('',#25611,#3101);
#1529=LINE('',#25614,#3102);
#1530=LINE('',#25616,#3103);
#1531=LINE('',#25619,#3104);
#1532=LINE('',#25621,#3105);
#1533=LINE('',#25624,#3106);
#1534=LINE('',#25626,#3107);
#1535=LINE('',#25634,#3108);
#1536=LINE('',#25637,#3109);
#1537=LINE('',#25645,#3110);
#1538=LINE('',#25717,#3111);
#1539=LINE('',#25720,#3112);
#1540=LINE('',#25732,#3113);
#1541=LINE('',#25735,#3114);
#1542=LINE('',#26145,#3115);
#1543=LINE('',#26148,#3116);
#1544=LINE('',#26156,#3117);
#1545=LINE('',#26228,#3118);
#1546=LINE('',#26231,#3119);
#1547=LINE('',#26247,#3120);
#1548=LINE('',#26250,#3121);
#1549=LINE('',#26318,#3122);
#1550=LINE('',#26344,#3123);
#1551=LINE('',#26350,#3124);
#1552=LINE('',#26353,#3125);
#1553=LINE('',#26359,#3126);
#1554=LINE('',#26362,#3127);
#1555=LINE('',#26388,#3128);
#1556=LINE('',#26562,#3129);
#1557=LINE('',#26568,#3130);
#1558=LINE('',#26571,#3131);
#1559=LINE('',#26577,#3132);
#1560=LINE('',#26580,#3133);
#1561=LINE('',#26586,#3134);
#1562=LINE('',#26589,#3135);
#1563=LINE('',#26593,#3136);
#1564=LINE('',#26595,#3137);
#1565=LINE('',#26600,#3138);
#1566=LINE('',#26607,#3139);
#1567=LINE('',#26809,#3140);
#1568=LINE('',#26812,#3141);
#1569=LINE('',#26818,#3142);
#1570=LINE('',#26823,#3143);
#1571=LINE('',#26843,#3144);
#1572=LINE('',#26845,#3145);
#1573=LINE('',#26849,#3146);
#1574=LINE('',#26851,#3147);
#1575=LINE('',#26852,#3148);
#1576=LINE('',#26854,#3149);
#1577=LINE('',#26856,#3150);
#1578=LINE('',#26858,#3151);
#1579=LINE('',#26862,#3152);
#1580=LINE('',#26864,#3153);
#1581=LINE('',#26866,#3154);
#1582=LINE('',#26870,#3155);
#1583=LINE('',#26872,#3156);
#1584=LINE('',#26874,#3157);
#1585=LINE('',#26878,#3158);
#1586=LINE('',#26880,#3159);
#1587=LINE('',#26882,#3160);
#1588=LINE('',#26884,#3161);
#1589=LINE('',#26888,#3162);
#1590=LINE('',#26890,#3163);
#1591=LINE('',#26892,#3164);
#1592=LINE('',#26894,#3165);
#1593=LINE('',#26896,#3166);
#1594=LINE('',#26900,#3167);
#1595=LINE('',#26902,#3168);
#1596=LINE('',#26904,#3169);
#1597=LINE('',#26908,#3170);
#1598=LINE('',#26910,#3171);
#1599=LINE('',#26912,#3172);
#1600=LINE('',#26915,#3173);
#1601=LINE('',#26918,#3174);
#1602=LINE('',#26921,#3175);
#1603=LINE('',#26924,#3176);
#1604=LINE('',#26927,#3177);
#1605=LINE('',#26930,#3178);
#1606=LINE('',#26933,#3179);
#1607=LINE('',#26936,#3180);
#1608=LINE('',#26939,#3181);
#1609=LINE('',#26942,#3182);
#1610=LINE('',#26945,#3183);
#1611=LINE('',#26948,#3184);
#1612=LINE('',#26950,#3185);
#1613=LINE('',#26954,#3186);
#1614=LINE('',#26957,#3187);
#1615=LINE('',#26960,#3188);
#1616=LINE('',#26963,#3189);
#1617=LINE('',#26968,#3190);
#1618=LINE('',#26971,#3191);
#1619=LINE('',#26975,#3192);
#1620=LINE('',#26981,#3193);
#1621=LINE('',#26985,#3194);
#1622=LINE('',#26989,#3195);
#1623=LINE('',#26995,#3196);
#1624=LINE('',#26997,#3197);
#1625=LINE('',#26998,#3198);
#1626=LINE('',#27001,#3199);
#1627=LINE('',#27003,#3200);
#1628=LINE('',#27004,#3201);
#1629=LINE('',#27006,#3202);
#1630=LINE('',#27008,#3203);
#1631=LINE('',#27009,#3204);
#1632=LINE('',#27011,#3205);
#1633=LINE('',#27013,#3206);
#1634=LINE('',#27014,#3207);
#1635=LINE('',#27016,#3208);
#1636=LINE('',#27018,#3209);
#1637=LINE('',#27020,#3210);
#1638=LINE('',#27022,#3211);
#1639=LINE('',#27023,#3212);
#1640=LINE('',#27025,#3213);
#1641=LINE('',#27027,#3214);
#1642=LINE('',#27029,#3215);
#1643=LINE('',#27030,#3216);
#1644=LINE('',#27032,#3217);
#1645=LINE('',#27034,#3218);
#1646=LINE('',#27035,#3219);
#1647=LINE('',#27037,#3220);
#1648=LINE('',#27039,#3221);
#1649=LINE('',#27040,#3222);
#1650=LINE('',#27042,#3223);
#1651=LINE('',#27044,#3224);
#1652=LINE('',#27045,#3225);
#1653=LINE('',#27047,#3226);
#1654=LINE('',#27049,#3227);
#1655=LINE('',#27050,#3228);
#1656=LINE('',#27052,#3229);
#1657=LINE('',#27054,#3230);
#1658=LINE('',#27055,#3231);
#1659=LINE('',#27058,#3232);
#1660=LINE('',#27059,#3233);
#1661=LINE('',#27063,#3234);
#1662=LINE('',#27064,#3235);
#1663=LINE('',#27068,#3236);
#1664=LINE('',#27070,#3237);
#1665=LINE('',#27072,#3238);
#1666=LINE('',#27073,#3239);
#1667=LINE('',#27077,#3240);
#1668=LINE('',#27079,#3241);
#1669=LINE('',#27080,#3242);
#1670=LINE('',#27084,#3243);
#1671=LINE('',#27085,#3244);
#1672=LINE('',#27089,#3245);
#1673=LINE('',#27090,#3246);
#1674=LINE('',#27094,#3247);
#1675=LINE('',#27095,#3248);
#1676=LINE('',#27099,#3249);
#1677=LINE('',#27100,#3250);
#1678=LINE('',#27104,#3251);
#1679=LINE('',#27105,#3252);
#1680=LINE('',#27155,#3253);
#1681=LINE('',#27157,#3254);
#1682=LINE('',#28379,#3255);
#1683=LINE('',#28384,#3256);
#1684=LINE('',#29077,#3257);
#1685=LINE('',#29080,#3258);
#1686=LINE('',#30305,#3259);
#1687=LINE('',#30311,#3260);
#1688=LINE('',#30317,#3261);
#1689=LINE('',#30323,#3262);
#1690=LINE('',#30328,#3263);
#1691=LINE('',#30330,#3264);
#1692=LINE('',#30332,#3265);
#1693=LINE('',#30334,#3266);
#1694=LINE('',#30336,#3267);
#1695=LINE('',#30338,#3268);
#1696=LINE('',#30340,#3269);
#1697=LINE('',#30342,#3270);
#1698=LINE('',#30344,#3271);
#1699=LINE('',#30346,#3272);
#1700=LINE('',#30348,#3273);
#1701=LINE('',#30349,#3274);
#1702=LINE('',#30353,#3275);
#1703=LINE('',#30355,#3276);
#1704=LINE('',#30357,#3277);
#1705=LINE('',#30359,#3278);
#1706=LINE('',#30361,#3279);
#1707=LINE('',#30363,#3280);
#1708=LINE('',#30365,#3281);
#1709=LINE('',#30367,#3282);
#1710=LINE('',#30369,#3283);
#1711=LINE('',#30371,#3284);
#1712=LINE('',#30373,#3285);
#1713=LINE('',#30374,#3286);
#1714=LINE('',#30377,#3287);
#1715=LINE('',#30379,#3288);
#1716=LINE('',#30380,#3289);
#1717=LINE('',#30383,#3290);
#1718=LINE('',#30385,#3291);
#1719=LINE('',#30386,#3292);
#1720=LINE('',#30389,#3293);
#1721=LINE('',#30391,#3294);
#1722=LINE('',#30392,#3295);
#1723=LINE('',#30395,#3296);
#1724=LINE('',#30397,#3297);
#1725=LINE('',#30398,#3298);
#1726=LINE('',#30400,#3299);
#1727=LINE('',#30401,#3300);
#1728=LINE('',#30404,#3301);
#1729=LINE('',#30406,#3302);
#1730=LINE('',#30407,#3303);
#1731=LINE('',#30410,#3304);
#1732=LINE('',#30412,#3305);
#1733=LINE('',#30413,#3306);
#1734=LINE('',#30416,#3307);
#1735=LINE('',#30418,#3308);
#1736=LINE('',#30419,#3309);
#1737=LINE('',#30422,#3310);
#1738=LINE('',#30424,#3311);
#1739=LINE('',#30425,#3312);
#1740=LINE('',#30427,#3313);
#1741=LINE('',#30428,#3314);
#1742=LINE('',#30432,#3315);
#1743=LINE('',#30434,#3316);
#1744=LINE('',#30435,#3317);
#1745=LINE('',#30437,#3318);
#1746=LINE('',#30439,#3319);
#1747=LINE('',#30440,#3320);
#1748=LINE('',#30443,#3321);
#1749=LINE('',#30444,#3322);
#1750=LINE('',#30447,#3323);
#1751=LINE('',#30448,#3324);
#1752=LINE('',#30450,#3325);
#1753=LINE('',#30452,#3326);
#1754=LINE('',#30454,#3327);
#1755=LINE('',#30456,#3328);
#1756=LINE('',#30457,#3329);
#1757=LINE('',#30460,#3330);
#1758=LINE('',#30461,#3331);
#1759=LINE('',#30462,#3332);
#1760=LINE('',#30464,#3333);
#1761=LINE('',#30465,#3334);
#1762=LINE('',#30468,#3335);
#1763=LINE('',#30469,#3336);
#1764=LINE('',#30471,#3337);
#1765=LINE('',#30475,#3338);
#1766=LINE('',#30476,#3339);
#1767=LINE('',#30479,#3340);
#1768=LINE('',#30480,#3341);
#1769=LINE('',#30482,#3342);
#1770=LINE('',#30484,#3343);
#1771=LINE('',#30487,#3344);
#1772=LINE('',#30494,#3345);
#1773=LINE('',#30500,#3346);
#1774=LINE('',#30506,#3347);
#1775=LINE('',#30512,#3348);
#1776=LINE('',#30518,#3349);
#1777=LINE('',#30524,#3350);
#1778=LINE('',#30530,#3351);
#1779=LINE('',#30536,#3352);
#1780=LINE('',#30542,#3353);
#1781=LINE('',#30548,#3354);
#1782=LINE('',#30554,#3355);
#1783=LINE('',#30560,#3356);
#1784=LINE('',#30566,#3357);
#1785=LINE('',#30572,#3358);
#1786=LINE('',#30578,#3359);
#1787=LINE('',#30584,#3360);
#1788=LINE('',#30590,#3361);
#1789=LINE('',#30598,#3362);
#1790=LINE('',#30645,#3363);
#1791=LINE('',#30648,#3364);
#1792=LINE('',#30651,#3365);
#1793=LINE('',#30654,#3366);
#1794=LINE('',#30656,#3367);
#1795=LINE('',#30665,#3368);
#1796=LINE('',#30669,#3369);
#1797=LINE('',#30675,#3370);
#1798=LINE('',#30681,#3371);
#1799=LINE('',#30683,#3372);
#1800=LINE('',#30685,#3373);
#1801=LINE('',#30687,#3374);
#1802=LINE('',#30689,#3375);
#1803=LINE('',#30690,#3376);
#1804=LINE('',#30693,#3377);
#1805=LINE('',#30695,#3378);
#1806=LINE('',#30696,#3379);
#1807=LINE('',#30699,#3380);
#1808=LINE('',#30700,#3381);
#1809=LINE('',#30703,#3382);
#1810=LINE('',#30705,#3383);
#1811=LINE('',#30706,#3384);
#1812=LINE('',#30709,#3385);
#1813=LINE('',#30710,#3386);
#1814=LINE('',#30713,#3387);
#1815=LINE('',#30714,#3388);
#1816=LINE('',#30717,#3389);
#1817=LINE('',#30718,#3390);
#1818=LINE('',#30720,#3391);
#1819=LINE('',#30737,#3392);
#1820=LINE('',#30752,#3393);
#1821=LINE('',#30767,#3394);
#1822=LINE('',#30800,#3395);
#1823=LINE('',#30806,#3396);
#1824=LINE('',#30812,#3397);
#1825=LINE('',#30818,#3398);
#1826=LINE('',#30827,#3399);
#1827=LINE('',#30887,#3400);
#1828=LINE('',#30893,#3401);
#1829=LINE('',#30936,#3402);
#1830=LINE('',#30945,#3403);
#1831=LINE('',#30951,#3404);
#1832=LINE('',#30975,#3405);
#1833=LINE('',#30995,#3406);
#1834=LINE('',#31018,#3407);
#1835=LINE('',#31038,#3408);
#1836=LINE('',#31051,#3409);
#1837=LINE('',#31071,#3410);
#1838=LINE('',#31102,#3411);
#1839=LINE('',#31105,#3412);
#1840=LINE('',#31128,#3413);
#1841=LINE('',#31148,#3414);
#1842=LINE('',#31156,#3415);
#1843=LINE('',#31159,#3416);
#1844=LINE('',#31164,#3417);
#1845=LINE('',#31170,#3418);
#1846=LINE('',#31176,#3419);
#1847=LINE('',#31182,#3420);
#1848=LINE('',#31188,#3421);
#1849=LINE('',#31195,#3422);
#1850=LINE('',#31215,#3423);
#1851=LINE('',#31221,#3424);
#1852=LINE('',#31243,#3425);
#1853=LINE('',#31248,#3426);
#1854=LINE('',#31264,#3427);
#1855=LINE('',#31293,#3428);
#1856=LINE('',#31367,#3429);
#1857=LINE('',#31376,#3430);
#1858=LINE('',#31379,#3431);
#1859=LINE('',#31385,#3432);
#1860=LINE('',#31388,#3433);
#1861=LINE('',#31390,#3434);
#1862=LINE('',#31393,#3435);
#1863=LINE('',#31396,#3436);
#1864=LINE('',#31402,#3437);
#1865=LINE('',#31408,#3438);
#1866=LINE('',#31414,#3439);
#1867=LINE('',#31420,#3440);
#1868=LINE('',#31426,#3441);
#1869=LINE('',#31430,#3442);
#1870=LINE('',#31434,#3443);
#1871=LINE('',#31439,#3444);
#1872=LINE('',#31445,#3445);
#1873=LINE('',#31451,#3446);
#1874=LINE('',#31455,#3447);
#1875=LINE('',#31461,#3448);
#1876=LINE('',#31467,#3449);
#1877=LINE('',#31473,#3450);
#1878=LINE('',#31479,#3451);
#1879=LINE('',#31485,#3452);
#1880=LINE('',#31491,#3453);
#1881=LINE('',#31498,#3454);
#1882=LINE('',#31501,#3455);
#1883=LINE('',#31504,#3456);
#1884=LINE('',#31513,#3457);
#1885=LINE('',#31516,#3458);
#1886=LINE('',#31522,#3459);
#1887=LINE('',#31528,#3460);
#1888=LINE('',#31593,#3461);
#1889=LINE('',#31597,#3462);
#1890=LINE('',#31649,#3463);
#1891=LINE('',#31655,#3464);
#1892=LINE('',#31659,#3465);
#1893=LINE('',#31665,#3466);
#1894=LINE('',#31674,#3467);
#1895=LINE('',#31677,#3468);
#1896=LINE('',#31680,#3469);
#1897=LINE('',#31730,#3470);
#1898=LINE('',#31786,#3471);
#1899=LINE('',#31803,#3472);
#1900=LINE('',#31818,#3473);
#1901=LINE('',#31862,#3474);
#1902=LINE('',#31864,#3475);
#1903=LINE('',#31936,#3476);
#1904=LINE('',#31938,#3477);
#1905=LINE('',#32025,#3478);
#1906=LINE('',#32027,#3479);
#1907=LINE('',#32029,#3480);
#1908=LINE('',#32031,#3481);
#1909=LINE('',#32033,#3482);
#1910=LINE('',#32034,#3483);
#1911=LINE('',#32038,#3484);
#1912=LINE('',#32040,#3485);
#1913=LINE('',#32042,#3486);
#1914=LINE('',#32044,#3487);
#1915=LINE('',#32046,#3488);
#1916=LINE('',#32047,#3489);
#1917=LINE('',#32051,#3490);
#1918=LINE('',#32053,#3491);
#1919=LINE('',#32055,#3492);
#1920=LINE('',#32057,#3493);
#1921=LINE('',#32059,#3494);
#1922=LINE('',#32060,#3495);
#1923=LINE('',#32064,#3496);
#1924=LINE('',#32066,#3497);
#1925=LINE('',#32068,#3498);
#1926=LINE('',#32070,#3499);
#1927=LINE('',#32072,#3500);
#1928=LINE('',#32073,#3501);
#1929=LINE('',#32079,#3502);
#1930=LINE('',#32087,#3503);
#1931=LINE('',#32092,#3504);
#1932=LINE('',#32100,#3505);
#1933=LINE('',#32107,#3506);
#1934=LINE('',#32109,#3507);
#1935=LINE('',#32111,#3508);
#1936=LINE('',#32113,#3509);
#1937=LINE('',#32115,#3510);
#1938=LINE('',#32116,#3511);
#1939=LINE('',#32120,#3512);
#1940=LINE('',#32122,#3513);
#1941=LINE('',#32124,#3514);
#1942=LINE('',#32126,#3515);
#1943=LINE('',#32128,#3516);
#1944=LINE('',#32129,#3517);
#1945=LINE('',#32133,#3518);
#1946=LINE('',#32134,#3519);
#1947=LINE('',#32135,#3520);
#1948=LINE('',#32138,#3521);
#1949=LINE('',#32139,#3522);
#1950=LINE('',#32142,#3523);
#1951=LINE('',#32143,#3524);
#1952=LINE('',#32146,#3525);
#1953=LINE('',#32147,#3526);
#1954=LINE('',#32150,#3527);
#1955=LINE('',#32151,#3528);
#1956=LINE('',#32153,#3529);
#1957=LINE('',#32157,#3530);
#1958=LINE('',#32159,#3531);
#1959=LINE('',#32161,#3532);
#1960=LINE('',#32163,#3533);
#1961=LINE('',#32168,#3534);
#1962=LINE('',#32173,#3535);
#1963=LINE('',#32175,#3536);
#1964=LINE('',#32177,#3537);
#1965=LINE('',#32182,#3538);
#1966=LINE('',#32183,#3539);
#1967=LINE('',#32184,#3540);
#1968=LINE('',#32187,#3541);
#1969=LINE('',#32188,#3542);
#1970=LINE('',#32191,#3543);
#1971=LINE('',#32192,#3544);
#1972=LINE('',#32195,#3545);
#1973=LINE('',#32196,#3546);
#1974=LINE('',#32199,#3547);
#1975=LINE('',#32200,#3548);
#1976=LINE('',#32202,#3549);
#1977=LINE('',#32206,#3550);
#1978=LINE('',#32208,#3551);
#1979=LINE('',#32210,#3552);
#1980=LINE('',#32212,#3553);
#1981=LINE('',#32217,#3554);
#1982=LINE('',#32223,#3555);
#1983=LINE('',#32224,#3556);
#1984=LINE('',#32226,#3557);
#1985=LINE('',#32231,#3558);
#1986=LINE('',#32232,#3559);
#1987=LINE('',#32233,#3560);
#1988=LINE('',#32236,#3561);
#1989=LINE('',#32237,#3562);
#1990=LINE('',#32240,#3563);
#1991=LINE('',#32241,#3564);
#1992=LINE('',#32244,#3565);
#1993=LINE('',#32245,#3566);
#1994=LINE('',#32248,#3567);
#1995=LINE('',#32249,#3568);
#1996=LINE('',#32251,#3569);
#1997=LINE('',#32255,#3570);
#1998=LINE('',#32257,#3571);
#1999=LINE('',#32259,#3572);
#2000=LINE('',#32261,#3573);
#2001=LINE('',#32266,#3574);
#2002=LINE('',#32272,#3575);
#2003=LINE('',#32273,#3576);
#2004=LINE('',#32275,#3577);
#2005=LINE('',#32278,#3578);
#2006=LINE('',#32280,#3579);
#2007=LINE('',#32282,#3580);
#2008=LINE('',#32286,#3581);
#2009=LINE('',#32287,#3582);
#2010=LINE('',#32288,#3583);
#2011=LINE('',#32292,#3584);
#2012=LINE('',#32293,#3585);
#2013=LINE('',#32294,#3586);
#2014=LINE('',#32297,#3587);
#2015=LINE('',#32298,#3588);
#2016=LINE('',#32301,#3589);
#2017=LINE('',#32302,#3590);
#2018=LINE('',#32305,#3591);
#2019=LINE('',#32306,#3592);
#2020=LINE('',#32309,#3593);
#2021=LINE('',#32310,#3594);
#2022=LINE('',#32312,#3595);
#2023=LINE('',#32315,#3596);
#2024=LINE('',#32317,#3597);
#2025=LINE('',#32319,#3598);
#2026=LINE('',#32323,#3599);
#2027=LINE('',#32328,#3600);
#2028=LINE('',#32329,#3601);
#2029=LINE('',#32333,#3602);
#2030=LINE('',#32335,#3603);
#2031=LINE('',#32339,#3604);
#2032=LINE('',#32340,#3605);
#2033=LINE('',#32343,#3606);
#2034=LINE('',#32347,#3607);
#2035=LINE('',#32351,#3608);
#2036=LINE('',#32355,#3609);
#2037=LINE('',#32356,#3610);
#2038=LINE('',#32359,#3611);
#2039=LINE('',#32363,#3612);
#2040=LINE('',#32367,#3613);
#2041=LINE('',#32371,#3614);
#2042=LINE('',#32372,#3615);
#2043=LINE('',#32377,#3616);
#2044=LINE('',#32381,#3617);
#2045=LINE('',#32382,#3618);
#2046=LINE('',#32385,#3619);
#2047=LINE('',#32391,#3620);
#2048=LINE('',#32393,#3621);
#2049=LINE('',#32397,#3622);
#2050=LINE('',#32401,#3623);
#2051=LINE('',#32405,#3624);
#2052=LINE('',#32409,#3625);
#2053=LINE('',#32415,#3626);
#2054=LINE('',#32417,#3627);
#2055=LINE('',#32421,#3628);
#2056=LINE('',#32425,#3629);
#2057=LINE('',#32429,#3630);
#2058=LINE('',#32433,#3631);
#2059=LINE('',#32438,#3632);
#2060=LINE('',#32440,#3633);
#2061=LINE('',#32445,#3634);
#2062=LINE('',#32446,#3635);
#2063=LINE('',#32448,#3636);
#2064=LINE('',#32451,#3637);
#2065=LINE('',#32454,#3638);
#2066=LINE('',#32457,#3639);
#2067=LINE('',#32460,#3640);
#2068=LINE('',#32462,#3641);
#2069=LINE('',#32465,#3642);
#2070=LINE('',#32468,#3643);
#2071=LINE('',#32479,#3644);
#2072=LINE('',#32481,#3645);
#2073=LINE('',#32492,#3646);
#2074=LINE('',#32501,#3647);
#2075=LINE('',#32517,#3648);
#2076=LINE('',#32519,#3649);
#2077=LINE('',#32530,#3650);
#2078=LINE('',#32544,#3651);
#2079=LINE('',#32547,#3652);
#2080=LINE('',#32548,#3653);
#2081=LINE('',#32552,#3654);
#2082=LINE('',#32554,#3655);
#2083=LINE('',#32569,#3656);
#2084=LINE('',#32571,#3657);
#2085=LINE('',#32582,#3658);
#2086=LINE('',#32598,#3659);
#2087=LINE('',#32888,#3660);
#2088=LINE('',#32889,#3661);
#2089=LINE('',#32892,#3662);
#2090=LINE('',#32893,#3663);
#2091=LINE('',#32897,#3664);
#2092=LINE('',#32900,#3665);
#2093=LINE('',#32901,#3666);
#2094=LINE('',#32905,#3667);
#2095=LINE('',#32908,#3668);
#2096=LINE('',#32909,#3669);
#2097=LINE('',#32913,#3670);
#2098=LINE('',#32915,#3671);
#2099=LINE('',#32924,#3672);
#2100=LINE('',#32925,#3673);
#2101=LINE('',#32966,#3674);
#2102=LINE('',#33001,#3675);
#2103=LINE('',#33058,#3676);
#2104=LINE('',#33074,#3677);
#2105=LINE('',#33102,#3678);
#2106=LINE('',#33124,#3679);
#2107=LINE('',#33154,#3680);
#2108=LINE('',#33176,#3681);
#2109=LINE('',#33415,#3682);
#2110=LINE('',#33431,#3683);
#2111=LINE('',#33440,#3684);
#2112=LINE('',#33456,#3685);
#2113=LINE('',#33465,#3686);
#2114=LINE('',#33635,#3687);
#2115=LINE('',#33707,#3688);
#2116=LINE('',#33789,#3689);
#2117=LINE('',#33867,#3690);
#2118=LINE('',#33949,#3691);
#2119=LINE('',#34027,#3692);
#2120=LINE('',#35967,#3693);
#2121=LINE('',#35986,#3694);
#2122=LINE('',#36078,#3695);
#2123=LINE('',#36094,#3696);
#2124=LINE('',#36124,#3697);
#2125=LINE('',#36146,#3698);
#2126=LINE('',#36176,#3699);
#2127=LINE('',#36198,#3700);
#2128=LINE('',#36232,#3701);
#2129=LINE('',#36236,#3702);
#2130=LINE('',#36240,#3703);
#2131=LINE('',#36244,#3704);
#2132=LINE('',#36250,#3705);
#2133=LINE('',#36251,#3706);
#2134=LINE('',#36255,#3707);
#2135=LINE('',#36259,#3708);
#2136=LINE('',#36262,#3709);
#2137=LINE('',#36267,#3710);
#2138=LINE('',#36271,#3711);
#2139=LINE('',#36277,#3712);
#2140=LINE('',#36281,#3713);
#2141=LINE('',#36291,#3714);
#2142=LINE('',#36296,#3715);
#2143=LINE('',#36300,#3716);
#2144=LINE('',#36304,#3717);
#2145=LINE('',#36309,#3718);
#2146=LINE('',#36311,#3719);
#2147=LINE('',#36312,#3720);
#2148=LINE('',#36315,#3721);
#2149=LINE('',#36317,#3722);
#2150=LINE('',#36318,#3723);
#2151=LINE('',#36337,#3724);
#2152=LINE('',#36339,#3725);
#2153=LINE('',#36340,#3726);
#2154=LINE('',#36374,#3727);
#2155=LINE('',#36377,#3728);
#2156=LINE('',#36394,#3729);
#2157=LINE('',#36452,#3730);
#2158=LINE('',#36520,#3731);
#2159=LINE('',#36664,#3732);
#2160=LINE('',#36738,#3733);
#2161=LINE('',#36883,#3734);
#2162=LINE('',#36958,#3735);
#2163=LINE('',#37100,#3736);
#2164=LINE('',#37168,#3737);
#2165=LINE('',#37283,#3738);
#2166=LINE('',#37285,#3739);
#2167=LINE('',#37287,#3740);
#2168=LINE('',#37289,#3741);
#2169=LINE('',#37291,#3742);
#2170=LINE('',#37292,#3743);
#2171=LINE('',#37296,#3744);
#2172=LINE('',#37298,#3745);
#2173=LINE('',#37300,#3746);
#2174=LINE('',#37302,#3747);
#2175=LINE('',#37304,#3748);
#2176=LINE('',#37305,#3749);
#2177=LINE('',#37307,#3750);
#2178=LINE('',#37309,#3751);
#2179=LINE('',#37311,#3752);
#2180=LINE('',#37313,#3753);
#2181=LINE('',#37318,#3754);
#2182=LINE('',#37325,#3755);
#2183=LINE('',#37326,#3756);
#2184=LINE('',#37329,#3757);
#2185=LINE('',#37330,#3758);
#2186=LINE('',#37337,#3759);
#2187=LINE('',#37341,#3760);
#2188=LINE('',#37344,#3761);
#2189=LINE('',#37355,#3762);
#2190=LINE('',#37356,#3763);
#2191=LINE('',#37359,#3764);
#2192=LINE('',#37360,#3765);
#2193=LINE('',#37367,#3766);
#2194=LINE('',#37379,#3767);
#2195=LINE('',#37380,#3768);
#2196=LINE('',#37383,#3769);
#2197=LINE('',#37384,#3770);
#2198=LINE('',#37391,#3771);
#2199=LINE('',#37395,#3772);
#2200=LINE('',#37398,#3773);
#2201=LINE('',#37409,#3774);
#2202=LINE('',#37410,#3775);
#2203=LINE('',#37413,#3776);
#2204=LINE('',#37414,#3777);
#2205=LINE('',#37421,#3778);
#2206=LINE('',#37425,#3779);
#2207=LINE('',#37430,#3780);
#2208=LINE('',#37432,#3781);
#2209=LINE('',#37433,#3782);
#2210=LINE('',#37436,#3783);
#2211=LINE('',#37437,#3784);
#2212=LINE('',#37440,#3785);
#2213=LINE('',#37441,#3786);
#2214=LINE('',#37444,#3787);
#2215=LINE('',#37445,#3788);
#2216=LINE('',#37448,#3789);
#2217=LINE('',#37449,#3790);
#2218=LINE('',#37451,#3791);
#2219=LINE('',#37454,#3792);
#2220=LINE('',#37456,#3793);
#2221=LINE('',#37457,#3794);
#2222=LINE('',#37460,#3795);
#2223=LINE('',#37461,#3796);
#2224=LINE('',#37464,#3797);
#2225=LINE('',#37465,#3798);
#2226=LINE('',#37468,#3799);
#2227=LINE('',#37469,#3800);
#2228=LINE('',#37472,#3801);
#2229=LINE('',#37473,#3802);
#2230=LINE('',#37475,#3803);
#2231=LINE('',#37481,#3804);
#2232=LINE('',#37484,#3805);
#2233=LINE('',#37490,#3806);
#2234=LINE('',#37493,#3807);
#2235=LINE('',#37497,#3808);
#2236=LINE('',#37499,#3809);
#2237=LINE('',#37501,#3810);
#2238=LINE('',#37502,#3811);
#2239=LINE('',#37506,#3812);
#2240=LINE('',#37510,#3813);
#2241=LINE('',#37511,#3814);
#2242=LINE('',#37512,#3815);
#2243=LINE('',#37515,#3816);
#2244=LINE('',#37517,#3817);
#2245=LINE('',#37524,#3818);
#2246=LINE('',#37527,#3819);
#2247=LINE('',#37533,#3820);
#2248=LINE('',#37536,#3821);
#2249=LINE('',#37542,#3822);
#2250=LINE('',#37545,#3823);
#2251=LINE('',#37547,#3824);
#2252=LINE('',#37548,#3825);
#2253=LINE('',#37549,#3826);
#2254=LINE('',#37550,#3827);
#2255=LINE('',#37551,#3828);
#2256=LINE('',#37553,#3829);
#2257=LINE('',#37556,#3830);
#2258=LINE('',#37557,#3831);
#2259=LINE('',#37562,#3832);
#2260=LINE('',#37563,#3833);
#2261=LINE('',#37568,#3834);
#2262=LINE('',#37570,#3835);
#2263=LINE('',#37571,#3836);
#2264=LINE('',#37574,#3837);
#2265=LINE('',#37576,#3838);
#2266=LINE('',#37577,#3839);
#2267=LINE('',#37580,#3840);
#2268=LINE('',#37584,#3841);
#2269=LINE('',#37586,#3842);
#2270=LINE('',#37588,#3843);
#2271=LINE('',#37591,#3844);
#2272=LINE('',#37595,#3845);
#2273=LINE('',#37599,#3846);
#2274=LINE('',#37603,#3847);
#2275=LINE('',#37605,#3848);
#2276=LINE('',#37607,#3849);
#2277=LINE('',#37608,#3850);
#2278=LINE('',#37610,#3851);
#2279=LINE('',#37611,#3852);
#2280=LINE('',#37615,#3853);
#2281=LINE('',#37618,#3854);
#2282=LINE('',#37619,#3855);
#2283=LINE('',#37622,#3856);
#2284=LINE('',#37623,#3857);
#2285=LINE('',#37627,#3858);
#2286=LINE('',#37628,#3859);
#2287=LINE('',#37630,#3860);
#2288=LINE('',#37631,#3861);
#2289=LINE('',#37634,#3862);
#2290=LINE('',#37636,#3863);
#2291=LINE('',#37637,#3864);
#2292=LINE('',#37641,#3865);
#2293=LINE('',#37642,#3866);
#2294=LINE('',#37643,#3867);
#2295=LINE('',#37646,#3868);
#2296=LINE('',#37649,#3869);
#2297=LINE('',#37653,#3870);
#2298=LINE('',#37657,#3871);
#2299=LINE('',#37661,#3872);
#2300=LINE('',#37663,#3873);
#2301=LINE('',#37664,#3874);
#2302=LINE('',#37666,#3875);
#2303=LINE('',#37667,#3876);
#2304=LINE('',#37670,#3877);
#2305=LINE('',#37672,#3878);
#2306=LINE('',#37673,#3879);
#2307=LINE('',#37676,#3880);
#2308=LINE('',#37680,#3881);
#2309=LINE('',#37682,#3882);
#2310=LINE('',#37684,#3883);
#2311=LINE('',#37687,#3884);
#2312=LINE('',#37691,#3885);
#2313=LINE('',#37695,#3886);
#2314=LINE('',#37699,#3887);
#2315=LINE('',#37701,#3888);
#2316=LINE('',#37702,#3889);
#2317=LINE('',#37704,#3890);
#2318=LINE('',#37705,#3891);
#2319=LINE('',#37709,#3892);
#2320=LINE('',#37713,#3893);
#2321=LINE('',#37716,#3894);
#2322=LINE('',#37718,#3895);
#2323=LINE('',#37719,#3896);
#2324=LINE('',#37722,#3897);
#2325=LINE('',#37723,#3898);
#2326=LINE('',#37726,#3899);
#2327=LINE('',#37730,#3900);
#2328=LINE('',#37732,#3901);
#2329=LINE('',#37734,#3902);
#2330=LINE('',#37737,#3903);
#2331=LINE('',#37741,#3904);
#2332=LINE('',#37743,#3905);
#2333=LINE('',#37745,#3906);
#2334=LINE('',#37747,#3907);
#2335=LINE('',#37749,#3908);
#2336=LINE('',#37750,#3909);
#2337=LINE('',#37754,#3910);
#2338=LINE('',#37756,#3911);
#2339=LINE('',#37758,#3912);
#2340=LINE('',#37759,#3913);
#2341=LINE('',#37764,#3914);
#2342=LINE('',#37765,#3915);
#2343=LINE('',#37767,#3916);
#2344=LINE('',#37769,#3917);
#2345=LINE('',#37773,#3918);
#2346=LINE('',#37776,#3919);
#2347=LINE('',#37779,#3920);
#2348=LINE('',#37781,#3921);
#2349=LINE('',#37782,#3922);
#2350=LINE('',#37785,#3923);
#2351=LINE('',#37789,#3924);
#2352=LINE('',#37790,#3925);
#2353=LINE('',#37793,#3926);
#2354=LINE('',#37794,#3927);
#2355=LINE('',#37797,#3928);
#2356=LINE('',#37798,#3929);
#2357=LINE('',#37801,#3930);
#2358=LINE('',#37805,#3931);
#2359=LINE('',#37807,#3932);
#2360=LINE('',#37808,#3933);
#2361=LINE('',#37811,#3934);
#2362=LINE('',#37813,#3935);
#2363=LINE('',#37815,#3936);
#2364=LINE('',#37819,#3937);
#2365=LINE('',#37822,#3938);
#2366=LINE('',#37825,#3939);
#2367=LINE('',#37827,#3940);
#2368=LINE('',#37828,#3941);
#2369=LINE('',#37831,#3942);
#2370=LINE('',#37835,#3943);
#2371=LINE('',#37836,#3944);
#2372=LINE('',#37839,#3945);
#2373=LINE('',#37840,#3946);
#2374=LINE('',#37843,#3947);
#2375=LINE('',#37844,#3948);
#2376=LINE('',#37847,#3949);
#2377=LINE('',#37851,#3950);
#2378=LINE('',#37853,#3951);
#2379=LINE('',#37854,#3952);
#2380=LINE('',#37857,#3953);
#2381=LINE('',#37859,#3954);
#2382=LINE('',#37861,#3955);
#2383=LINE('',#37865,#3956);
#2384=LINE('',#37868,#3957);
#2385=LINE('',#37871,#3958);
#2386=LINE('',#37873,#3959);
#2387=LINE('',#37874,#3960);
#2388=LINE('',#37877,#3961);
#2389=LINE('',#37881,#3962);
#2390=LINE('',#37882,#3963);
#2391=LINE('',#37885,#3964);
#2392=LINE('',#37886,#3965);
#2393=LINE('',#37889,#3966);
#2394=LINE('',#37890,#3967);
#2395=LINE('',#37893,#3968);
#2396=LINE('',#37897,#3969);
#2397=LINE('',#37899,#3970);
#2398=LINE('',#37900,#3971);
#2399=LINE('',#37903,#3972);
#2400=LINE('',#37905,#3973);
#2401=LINE('',#37907,#3974);
#2402=LINE('',#37911,#3975);
#2403=LINE('',#37914,#3976);
#2404=LINE('',#37917,#3977);
#2405=LINE('',#37919,#3978);
#2406=LINE('',#37920,#3979);
#2407=LINE('',#37923,#3980);
#2408=LINE('',#37927,#3981);
#2409=LINE('',#37928,#3982);
#2410=LINE('',#37931,#3983);
#2411=LINE('',#37932,#3984);
#2412=LINE('',#37935,#3985);
#2413=LINE('',#37936,#3986);
#2414=LINE('',#37939,#3987);
#2415=LINE('',#37943,#3988);
#2416=LINE('',#37944,#3989);
#2417=LINE('',#37947,#3990);
#2418=LINE('',#37949,#3991);
#2419=LINE('',#37950,#3992);
#2420=LINE('',#37953,#3993);
#2421=LINE('',#37954,#3994);
#2422=LINE('',#37957,#3995);
#2423=LINE('',#37958,#3996);
#2424=LINE('',#37961,#3997);
#2425=LINE('',#37962,#3998);
#2426=LINE('',#37965,#3999);
#2427=LINE('',#37966,#4000);
#2428=LINE('',#37968,#4001);
#2429=LINE('',#37972,#4002);
#2430=LINE('',#37973,#4003);
#2431=LINE('',#37975,#4004);
#2432=LINE('',#37977,#4005);
#2433=LINE('',#37985,#4006);
#2434=LINE('',#37987,#4007);
#2435=LINE('',#37988,#4008);
#2436=LINE('',#37992,#4009);
#2437=LINE('',#37996,#4010);
#2438=LINE('',#37999,#4011);
#2439=LINE('',#38003,#4012);
#2440=LINE('',#38004,#4013);
#2441=LINE('',#38007,#4014);
#2442=LINE('',#38011,#4015);
#2443=LINE('',#38012,#4016);
#2444=LINE('',#38015,#4017);
#2445=LINE('',#38019,#4018);
#2446=LINE('',#38021,#4019);
#2447=LINE('',#38023,#4020);
#2448=LINE('',#38025,#4021);
#2449=LINE('',#38027,#4022);
#2450=LINE('',#38030,#4023);
#2451=LINE('',#38034,#4024);
#2452=LINE('',#38037,#4025);
#2453=LINE('',#38040,#4026);
#2454=LINE('',#38041,#4027);
#2455=LINE('',#38044,#4028);
#2456=LINE('',#38048,#4029);
#2457=LINE('',#38049,#4030);
#2458=LINE('',#38052,#4031);
#2459=LINE('',#38056,#4032);
#2460=LINE('',#38060,#4033);
#2461=LINE('',#38064,#4034);
#2462=LINE('',#38065,#4035);
#2463=LINE('',#38072,#4036);
#2464=LINE('',#38074,#4037);
#2465=LINE('',#38076,#4038);
#2466=LINE('',#38078,#4039);
#2467=LINE('',#38080,#4040);
#2468=LINE('',#38081,#4041);
#2469=LINE('',#38083,#4042);
#2470=LINE('',#38084,#4043);
#2471=LINE('',#38086,#4044);
#2472=LINE('',#38088,#4045);
#2473=LINE('',#38090,#4046);
#2474=LINE('',#38092,#4047);
#2475=LINE('',#38094,#4048);
#2476=LINE('',#38097,#4049);
#2477=LINE('',#38099,#4050);
#2478=LINE('',#38101,#4051);
#2479=LINE('',#38103,#4052);
#2480=LINE('',#38105,#4053);
#2481=LINE('',#38107,#4054);
#2482=LINE('',#38109,#4055);
#2483=LINE('',#38114,#4056);
#2484=LINE('',#38116,#4057);
#2485=LINE('',#38118,#4058);
#2486=LINE('',#38120,#4059);
#2487=LINE('',#38122,#4060);
#2488=LINE('',#38124,#4061);
#2489=LINE('',#38126,#4062);
#2490=LINE('',#38127,#4063);
#2491=LINE('',#38135,#4064);
#2492=LINE('',#38140,#4065);
#2493=LINE('',#38142,#4066);
#2494=LINE('',#38144,#4067);
#2495=LINE('',#38146,#4068);
#2496=LINE('',#38148,#4069);
#2497=LINE('',#38149,#4070);
#2498=LINE('',#38150,#4071);
#2499=LINE('',#38154,#4072);
#2500=LINE('',#38156,#4073);
#2501=LINE('',#38158,#4074);
#2502=LINE('',#38160,#4075);
#2503=LINE('',#38162,#4076);
#2504=LINE('',#38163,#4077);
#2505=LINE('',#38177,#4078);
#2506=LINE('',#38179,#4079);
#2507=LINE('',#38180,#4080);
#2508=LINE('',#38183,#4081);
#2509=LINE('',#38184,#4082);
#2510=LINE('',#38187,#4083);
#2511=LINE('',#38188,#4084);
#2512=LINE('',#38191,#4085);
#2513=LINE('',#38192,#4086);
#2514=LINE('',#38195,#4087);
#2515=LINE('',#38196,#4088);
#2516=LINE('',#38198,#4089);
#2517=LINE('',#38201,#4090);
#2518=LINE('',#38204,#4091);
#2519=LINE('',#38219,#4092);
#2520=LINE('',#38220,#4093);
#2521=LINE('',#38224,#4094);
#2522=LINE('',#38226,#4095);
#2523=LINE('',#38228,#4096);
#2524=LINE('',#38230,#4097);
#2525=LINE('',#38232,#4098);
#2526=LINE('',#38233,#4099);
#2527=LINE('',#38237,#4100);
#2528=LINE('',#38239,#4101);
#2529=LINE('',#38241,#4102);
#2530=LINE('',#38243,#4103);
#2531=LINE('',#38245,#4104);
#2532=LINE('',#38246,#4105);
#2533=LINE('',#38250,#4106);
#2534=LINE('',#38252,#4107);
#2535=LINE('',#38254,#4108);
#2536=LINE('',#38256,#4109);
#2537=LINE('',#38258,#4110);
#2538=LINE('',#38259,#4111);
#2539=LINE('',#38263,#4112);
#2540=LINE('',#38266,#4113);
#2541=LINE('',#38267,#4114);
#2542=LINE('',#38273,#4115);
#2543=LINE('',#38276,#4116);
#2544=LINE('',#38277,#4117);
#2545=LINE('',#38286,#4118);
#2546=LINE('',#38289,#4119);
#2547=LINE('',#38290,#4120);
#2548=LINE('',#38296,#4121);
#2549=LINE('',#38299,#4122);
#2550=LINE('',#38300,#4123);
#2551=LINE('',#38305,#4124);
#2552=LINE('',#38307,#4125);
#2553=LINE('',#38308,#4126);
#2554=LINE('',#38311,#4127);
#2555=LINE('',#38312,#4128);
#2556=LINE('',#38315,#4129);
#2557=LINE('',#38316,#4130);
#2558=LINE('',#38319,#4131);
#2559=LINE('',#38320,#4132);
#2560=LINE('',#38323,#4133);
#2561=LINE('',#38324,#4134);
#2562=LINE('',#38326,#4135);
#2563=LINE('',#38331,#4136);
#2564=LINE('',#38332,#4137);
#2565=LINE('',#38344,#4138);
#2566=LINE('',#38347,#4139);
#2567=LINE('',#38350,#4140);
#2568=LINE('',#38364,#4141);
#2569=LINE('',#38366,#4142);
#2570=LINE('',#38368,#4143);
#2571=LINE('',#38370,#4144);
#2572=LINE('',#38372,#4145);
#2573=LINE('',#38373,#4146);
#2574=LINE('',#38377,#4147);
#2575=LINE('',#38379,#4148);
#2576=LINE('',#38381,#4149);
#2577=LINE('',#38383,#4150);
#2578=LINE('',#38385,#4151);
#2579=LINE('',#38386,#4152);
#2580=LINE('',#38390,#4153);
#2581=LINE('',#38392,#4154);
#2582=LINE('',#38394,#4155);
#2583=LINE('',#38396,#4156);
#2584=LINE('',#38398,#4157);
#2585=LINE('',#38399,#4158);
#2586=LINE('',#38402,#4159);
#2587=LINE('',#38403,#4160);
#2588=LINE('',#38406,#4161);
#2589=LINE('',#38407,#4162);
#2590=LINE('',#38409,#4163);
#2591=LINE('',#38413,#4164);
#2592=LINE('',#38415,#4165);
#2593=LINE('',#38417,#4166);
#2594=LINE('',#38419,#4167);
#2595=LINE('',#38421,#4168);
#2596=LINE('',#38422,#4169);
#2597=LINE('',#38426,#4170);
#2598=LINE('',#38428,#4171);
#2599=LINE('',#38430,#4172);
#2600=LINE('',#38432,#4173);
#2601=LINE('',#38434,#4174);
#2602=LINE('',#38435,#4175);
#2603=LINE('',#38438,#4176);
#2604=LINE('',#38440,#4177);
#2605=LINE('',#38441,#4178);
#2606=LINE('',#38444,#4179);
#2607=LINE('',#38445,#4180);
#2608=LINE('',#38448,#4181);
#2609=LINE('',#38449,#4182);
#2610=LINE('',#38452,#4183);
#2611=LINE('',#38453,#4184);
#2612=LINE('',#38456,#4185);
#2613=LINE('',#38457,#4186);
#2614=LINE('',#38459,#4187);
#2615=LINE('',#38463,#4188);
#2616=LINE('',#38466,#4189);
#2617=LINE('',#38470,#4190);
#2618=LINE('',#38475,#4191);
#2619=LINE('',#38477,#4192);
#2620=LINE('',#38480,#4193);
#2621=LINE('',#38483,#4194);
#2622=LINE('',#38485,#4195);
#2623=LINE('',#38486,#4196);
#2624=LINE('',#38489,#4197);
#2625=LINE('',#38490,#4198);
#2626=LINE('',#38493,#4199);
#2627=LINE('',#38494,#4200);
#2628=LINE('',#38497,#4201);
#2629=LINE('',#38498,#4202);
#2630=LINE('',#38501,#4203);
#2631=LINE('',#38502,#4204);
#2632=LINE('',#38504,#4205);
#2633=LINE('',#38508,#4206);
#2634=LINE('',#38512,#4207);
#2635=LINE('',#38516,#4208);
#2636=LINE('',#38520,#4209);
#2637=LINE('',#38521,#4210);
#2638=LINE('',#38524,#4211);
#2639=LINE('',#38526,#4212);
#2640=LINE('',#38527,#4213);
#2641=LINE('',#38530,#4214);
#2642=LINE('',#38531,#4215);
#2643=LINE('',#38534,#4216);
#2644=LINE('',#38535,#4217);
#2645=LINE('',#38538,#4218);
#2646=LINE('',#38539,#4219);
#2647=LINE('',#38542,#4220);
#2648=LINE('',#38543,#4221);
#2649=LINE('',#38545,#4222);
#2650=LINE('',#38549,#4223);
#2651=LINE('',#38617,#4224);
#2652=LINE('',#38619,#4225);
#2653=LINE('',#38633,#4226);
#2654=LINE('',#38634,#4227);
#2655=LINE('',#38637,#4228);
#2656=LINE('',#38709,#4229);
#2657=LINE('',#38717,#4230);
#2658=LINE('',#38718,#4231);
#2659=LINE('',#38719,#4232);
#2660=LINE('',#38722,#4233);
#2661=LINE('',#38846,#4234);
#2662=LINE('',#38848,#4235);
#2663=LINE('',#38850,#4236);
#2664=LINE('',#38853,#4237);
#2665=LINE('',#38855,#4238);
#2666=LINE('',#38860,#4239);
#2667=LINE('',#38862,#4240);
#2668=LINE('',#38865,#4241);
#2669=LINE('',#38871,#4242);
#2670=LINE('',#38872,#4243);
#2671=LINE('',#38875,#4244);
#2672=LINE('',#38878,#4245);
#2673=LINE('',#38879,#4246);
#2674=LINE('',#38882,#4247);
#2675=LINE('',#38884,#4248);
#2676=LINE('',#38885,#4249);
#2677=LINE('',#38888,#4250);
#2678=LINE('',#38889,#4251);
#2679=LINE('',#38892,#4252);
#2680=LINE('',#38893,#4253);
#2681=LINE('',#38896,#4254);
#2682=LINE('',#38897,#4255);
#2683=LINE('',#38900,#4256);
#2684=LINE('',#38901,#4257);
#2685=LINE('',#38903,#4258);
#2686=LINE('',#38980,#4259);
#2687=LINE('',#38983,#4260);
#2688=LINE('',#38986,#4261);
#2689=LINE('',#38990,#4262);
#2690=LINE('',#38992,#4263);
#2691=LINE('',#38996,#4264);
#2692=LINE('',#38998,#4265);
#2693=LINE('',#38999,#4266);
#2694=LINE('',#39002,#4267);
#2695=LINE('',#39003,#4268);
#2696=LINE('',#39006,#4269);
#2697=LINE('',#39007,#4270);
#2698=LINE('',#39010,#4271);
#2699=LINE('',#39011,#4272);
#2700=LINE('',#39014,#4273);
#2701=LINE('',#39015,#4274);
#2702=LINE('',#39017,#4275);
#2703=LINE('',#39020,#4276);
#2704=LINE('',#39022,#4277);
#2705=LINE('',#39023,#4278);
#2706=LINE('',#39026,#4279);
#2707=LINE('',#39027,#4280);
#2708=LINE('',#39030,#4281);
#2709=LINE('',#39031,#4282);
#2710=LINE('',#39034,#4283);
#2711=LINE('',#39035,#4284);
#2712=LINE('',#39038,#4285);
#2713=LINE('',#39039,#4286);
#2714=LINE('',#39041,#4287);
#2715=LINE('',#39046,#4288);
#2716=LINE('',#39048,#4289);
#2717=LINE('',#39050,#4290);
#2718=LINE('',#39052,#4291);
#2719=LINE('',#39054,#4292);
#2720=LINE('',#39055,#4293);
#2721=LINE('',#39060,#4294);
#2722=LINE('',#39062,#4295);
#2723=LINE('',#39064,#4296);
#2724=LINE('',#39066,#4297);
#2725=LINE('',#39068,#4298);
#2726=LINE('',#39069,#4299);
#2727=LINE('',#39073,#4300);
#2728=LINE('',#39074,#4301);
#2729=LINE('',#39075,#4302);
#2730=LINE('',#39078,#4303);
#2731=LINE('',#39080,#4304);
#2732=LINE('',#39082,#4305);
#2733=LINE('',#39084,#4306);
#2734=LINE('',#39085,#4307);
#2735=LINE('',#39089,#4308);
#2736=LINE('',#39090,#4309);
#2737=LINE('',#39091,#4310);
#2738=LINE('',#39094,#4311);
#2739=LINE('',#39096,#4312);
#2740=LINE('',#39097,#4313);
#2741=LINE('',#39100,#4314);
#2742=LINE('',#39101,#4315);
#2743=LINE('',#39104,#4316);
#2744=LINE('',#39105,#4317);
#2745=LINE('',#39108,#4318);
#2746=LINE('',#39109,#4319);
#2747=LINE('',#39112,#4320);
#2748=LINE('',#39113,#4321);
#2749=LINE('',#39115,#4322);
#2750=LINE('',#39121,#4323);
#2751=LINE('',#39122,#4324);
#2752=LINE('',#39124,#4325);
#2753=LINE('',#39125,#4326);
#2754=LINE('',#39128,#4327);
#2755=LINE('',#39129,#4328);
#2756=LINE('',#39132,#4329);
#2757=LINE('',#39133,#4330);
#2758=LINE('',#39136,#4331);
#2759=LINE('',#39138,#4332);
#2760=LINE('',#39141,#4333);
#2761=LINE('',#39144,#4334);
#2762=LINE('',#39145,#4335);
#2763=LINE('',#39147,#4336);
#2764=LINE('',#39150,#4337);
#2765=LINE('',#39154,#4338);
#2766=LINE('',#39233,#4339);
#2767=LINE('',#39235,#4340);
#2768=LINE('',#39239,#4341);
#2769=LINE('',#39242,#4342);
#2770=LINE('',#39319,#4343);
#2771=LINE('',#39321,#4344);
#2772=LINE('',#39322,#4345);
#2773=LINE('',#39327,#4346);
#2774=LINE('',#39328,#4347);
#2775=LINE('',#39331,#4348);
#2776=LINE('',#39332,#4349);
#2777=LINE('',#39334,#4350);
#2778=LINE('',#39337,#4351);
#2779=LINE('',#39342,#4352);
#2780=LINE('',#39346,#4353);
#2781=LINE('',#39350,#4354);
#2782=LINE('',#39352,#4355);
#2783=LINE('',#39353,#4356);
#2784=LINE('',#39356,#4357);
#2785=LINE('',#39357,#4358);
#2786=LINE('',#39360,#4359);
#2787=LINE('',#39361,#4360);
#2788=LINE('',#39364,#4361);
#2789=LINE('',#39365,#4362);
#2790=LINE('',#39368,#4363);
#2791=LINE('',#39369,#4364);
#2792=LINE('',#39371,#4365);
#2793=LINE('',#39373,#4366);
#2794=LINE('',#39375,#4367);
#2795=LINE('',#39379,#4368);
#2796=LINE('',#39380,#4369);
#2797=LINE('',#39381,#4370);
#2798=LINE('',#39384,#4371);
#2799=LINE('',#39385,#4372);
#2800=LINE('',#39388,#4373);
#2801=LINE('',#39389,#4374);
#2802=LINE('',#39391,#4375);
#2803=LINE('',#39393,#4376);
#2804=LINE('',#39396,#4377);
#2805=LINE('',#39398,#4378);
#2806=LINE('',#39399,#4379);
#2807=LINE('',#39403,#4380);
#2808=LINE('',#39408,#4381);
#2809=LINE('',#39411,#4382);
#2810=LINE('',#39414,#4383);
#2811=LINE('',#39415,#4384);
#2812=LINE('',#39420,#4385);
#2813=LINE('',#39424,#4386);
#2814=LINE('',#39425,#4387);
#2815=LINE('',#39430,#4388);
#2816=LINE('',#39433,#4389);
#2817=LINE('',#39434,#4390);
#2818=LINE('',#39436,#4391);
#2819=LINE('',#39440,#4392);
#2820=LINE('',#39445,#4393);
#2821=LINE('',#39489,#4394);
#2822=LINE('',#39490,#4395);
#2823=LINE('',#39492,#4396);
#2824=LINE('',#39494,#4397);
#2825=LINE('',#39496,#4398);
#2826=LINE('',#39497,#4399);
#2827=LINE('',#39500,#4400);
#2828=LINE('',#39501,#4401);
#2829=LINE('',#39504,#4402);
#2830=LINE('',#39506,#4403);
#2831=LINE('',#39507,#4404);
#2832=LINE('',#39510,#4405);
#2833=LINE('',#39511,#4406);
#2834=LINE('',#39514,#4407);
#2835=LINE('',#39516,#4408);
#2836=LINE('',#39517,#4409);
#2837=LINE('',#39520,#4410);
#2838=LINE('',#39521,#4411);
#2839=LINE('',#39525,#4412);
#2840=LINE('',#39527,#4413);
#2841=LINE('',#39529,#4414);
#2842=LINE('',#39531,#4415);
#2843=LINE('',#39533,#4416);
#2844=LINE('',#39534,#4417);
#2845=LINE('',#39536,#4418);
#2846=LINE('',#39538,#4419);
#2847=LINE('',#39540,#4420);
#2848=LINE('',#39541,#4421);
#2849=LINE('',#39544,#4422);
#2850=LINE('',#39545,#4423);
#2851=LINE('',#39549,#4424);
#2852=LINE('',#39550,#4425);
#2853=LINE('',#39551,#4426);
#2854=LINE('',#39554,#4427);
#2855=LINE('',#39555,#4428);
#2856=LINE('',#39559,#4429);
#2857=LINE('',#39560,#4430);
#2858=LINE('',#39561,#4431);
#2859=LINE('',#39564,#4432);
#2860=LINE('',#39565,#4433);
#2861=LINE('',#39569,#4434);
#2862=LINE('',#39570,#4435);
#2863=LINE('',#39572,#4436);
#2864=LINE('',#39574,#4437);
#2865=LINE('',#39575,#4438);
#2866=LINE('',#39579,#4439);
#2867=LINE('',#39580,#4440);
#2868=LINE('',#39581,#4441);
#2869=LINE('',#39585,#4442);
#2870=LINE('',#39586,#4443);
#2871=LINE('',#39591,#4444);
#2872=LINE('',#39592,#4445);
#2873=LINE('',#39597,#4446);
#2874=LINE('',#39598,#4447);
#2875=LINE('',#39601,#4448);
#2876=LINE('',#39602,#4449);
#2877=LINE('',#39603,#4450);
#2878=LINE('',#39605,#4451);
#2879=LINE('',#39606,#4452);
#2880=LINE('',#39607,#4453);
#2881=LINE('',#39610,#4454);
#2882=LINE('',#39611,#4455);
#2883=LINE('',#39613,#4456);
#2884=LINE('',#39615,#4457);
#2885=LINE('',#39618,#4458);
#2886=LINE('',#39619,#4459);
#2887=LINE('',#39622,#4460);
#2888=LINE('',#39623,#4461);
#2889=LINE('',#39625,#4462);
#2890=LINE('',#39627,#4463);
#2891=LINE('',#39628,#4464);
#2892=LINE('',#39630,#4465);
#2893=LINE('',#39631,#4466);
#2894=LINE('',#39660,#4467);
#2895=LINE('',#39662,#4468);
#2896=LINE('',#39663,#4469);
#2897=LINE('',#39664,#4470);
#2898=LINE('',#39667,#4471);
#2899=LINE('',#39669,#4472);
#2900=LINE('',#39670,#4473);
#2901=LINE('',#39673,#4474);
#2902=LINE('',#39674,#4475);
#2903=LINE('',#39676,#4476);
#2904=LINE('',#39678,#4477);
#2905=LINE('',#39680,#4478);
#2906=LINE('',#39681,#4479);
#2907=LINE('',#39685,#4480);
#2908=LINE('',#39686,#4481);
#2909=LINE('',#39687,#4482);
#2910=LINE('',#39690,#4483);
#2911=LINE('',#39691,#4484);
#2912=LINE('',#39694,#4485);
#2913=LINE('',#39695,#4486);
#2914=LINE('',#39698,#4487);
#2915=LINE('',#39700,#4488);
#2916=LINE('',#39701,#4489);
#2917=LINE('',#39705,#4490);
#2918=LINE('',#39706,#4491);
#2919=LINE('',#39707,#4492);
#2920=LINE('',#39710,#4493);
#2921=LINE('',#39711,#4494);
#2922=LINE('',#39714,#4495);
#2923=LINE('',#39715,#4496);
#2924=LINE('',#39717,#4497);
#2925=LINE('',#39719,#4498);
#2926=LINE('',#39721,#4499);
#2927=LINE('',#39725,#4500);
#2928=LINE('',#39726,#4501);
#2929=LINE('',#39728,#4502);
#2930=LINE('',#39729,#4503);
#2931=LINE('',#39732,#4504);
#2932=LINE('',#39733,#4505);
#2933=LINE('',#39736,#4506);
#2934=LINE('',#39738,#4507);
#2935=LINE('',#39739,#4508);
#2936=LINE('',#39742,#4509);
#2937=LINE('',#39744,#4510);
#2938=LINE('',#39745,#4511);
#2939=LINE('',#39748,#4512);
#2940=LINE('',#39749,#4513);
#2941=LINE('',#39752,#4514);
#2942=LINE('',#39753,#4515);
#2943=LINE('',#39756,#4516);
#2944=LINE('',#39757,#4517);
#2945=LINE('',#39760,#4518);
#2946=LINE('',#39761,#4519);
#2947=LINE('',#39764,#4520);
#2948=LINE('',#39765,#4521);
#2949=LINE('',#39768,#4522);
#2950=LINE('',#39769,#4523);
#2951=LINE('',#39772,#4524);
#2952=LINE('',#39773,#4525);
#2953=LINE('',#39776,#4526);
#2954=LINE('',#39777,#4527);
#2955=LINE('',#39780,#4528);
#2956=LINE('',#39781,#4529);
#2957=LINE('',#39784,#4530);
#2958=LINE('',#39785,#4531);
#2959=LINE('',#39787,#4532);
#2960=LINE('',#39807,#4533);
#2961=LINE('',#39818,#4534);
#2962=LINE('',#39821,#4535);
#2963=LINE('',#39826,#4536);
#2964=LINE('',#39827,#4537);
#2965=LINE('',#39830,#4538);
#2966=LINE('',#39831,#4539);
#2967=LINE('',#39834,#4540);
#2968=LINE('',#39835,#4541);
#2969=LINE('',#39838,#4542);
#2970=LINE('',#39839,#4543);
#2971=LINE('',#39842,#4544);
#2972=LINE('',#39843,#4545);
#2973=LINE('',#39846,#4546);
#2974=LINE('',#39847,#4547);
#2975=LINE('',#39910,#4548);
#2976=LINE('',#39911,#4549);
#2977=LINE('',#39913,#4550);
#2978=LINE('',#39915,#4551);
#2979=LINE('',#39917,#4552);
#2980=LINE('',#39919,#4553);
#2981=VECTOR('',#20036,1000.);
#2982=VECTOR('',#20039,1000.);
#2983=VECTOR('',#20042,1000.);
#2984=VECTOR('',#20045,1000.);
#2985=VECTOR('',#20048,1000.);
#2986=VECTOR('',#20051,1000.);
#2987=VECTOR('',#20054,1000.);
#2988=VECTOR('',#20057,1000.);
#2989=VECTOR('',#20060,35.);
#2990=VECTOR('',#20065,1000.);
#2991=VECTOR('',#20068,1000.);
#2992=VECTOR('',#20071,1000.);
#2993=VECTOR('',#20074,1000.);
#2994=VECTOR('',#20077,1000.);
#2995=VECTOR('',#20080,1000.);
#2996=VECTOR('',#20083,1000.);
#2997=VECTOR('',#20086,1000.);
#2998=VECTOR('',#20089,1000.);
#2999=VECTOR('',#20092,1000.);
#3000=VECTOR('',#20097,2.5);
#3001=VECTOR('',#20104,2.49999999999997);
#3002=VECTOR('',#20111,2.5);
#3003=VECTOR('',#20118,2.5);
#3004=VECTOR('',#20125,2.49999999999997);
#3005=VECTOR('',#20132,2.5);
#3006=VECTOR('',#20139,2.5);
#3007=VECTOR('',#20146,2.5);
#3008=VECTOR('',#20151,19.);
#3009=VECTOR('',#20156,19.);
#3010=VECTOR('',#20161,15.);
#3011=VECTOR('',#20166,15.);
#3012=VECTOR('',#20171,25.);
#3013=VECTOR('',#20178,2.5);
#3014=VECTOR('',#20185,2.5);
#3015=VECTOR('',#20192,2.5);
#3016=VECTOR('',#20199,2.5);
#3017=VECTOR('',#20206,2.5);
#3018=VECTOR('',#20213,2.5);
#3019=VECTOR('',#20220,2.5);
#3020=VECTOR('',#20227,2.5);
#3021=VECTOR('',#20234,2.50000000000001);
#3022=VECTOR('',#20241,2.5);
#3023=VECTOR('',#20248,2.5);
#3024=VECTOR('',#20255,2.5);
#3025=VECTOR('',#20262,2.5);
#3026=VECTOR('',#20269,2.5);
#3027=VECTOR('',#20276,2.5);
#3028=VECTOR('',#20281,250.);
#3029=VECTOR('',#20288,275.);
#3030=VECTOR('',#20295,240.);
#3031=VECTOR('',#20300,1000.);
#3032=VECTOR('',#20301,1000.);
#3033=VECTOR('',#20302,1000.);
#3034=VECTOR('',#20303,1000.);
#3035=VECTOR('',#20304,1000.);
#3036=VECTOR('',#20305,1000.);
#3037=VECTOR('',#20306,1000.);
#3038=VECTOR('',#20307,1000.);
#3039=VECTOR('',#20308,1000.);
#3040=VECTOR('',#20309,1000.);
#3041=VECTOR('',#20310,1000.);
#3042=VECTOR('',#20311,1000.);
#3043=VECTOR('',#20312,1000.);
#3044=VECTOR('',#20313,1000.);
#3045=VECTOR('',#20314,1000.);
#3046=VECTOR('',#20315,1000.);
#3047=VECTOR('',#20316,1000.);
#3048=VECTOR('',#20317,1000.);
#3049=VECTOR('',#20318,1000.);
#3050=VECTOR('',#20319,1000.);
#3051=VECTOR('',#20320,1000.);
#3052=VECTOR('',#20321,1000.);
#3053=VECTOR('',#20322,1000.);
#3054=VECTOR('',#20323,1000.);
#3055=VECTOR('',#20324,1000.);
#3056=VECTOR('',#20325,1000.);
#3057=VECTOR('',#20326,1000.);
#3058=VECTOR('',#20337,1000.);
#3059=VECTOR('',#20340,1000.);
#3060=VECTOR('',#20343,1000.);
#3061=VECTOR('',#20346,1000.);
#3062=VECTOR('',#20351,1000.);
#3063=VECTOR('',#20354,1000.);
#3064=VECTOR('',#20357,1000.);
#3065=VECTOR('',#20360,1000.);
#3066=VECTOR('',#20363,1000.);
#3067=VECTOR('',#20364,1000.);
#3068=VECTOR('',#20367,1000.);
#3069=VECTOR('',#20370,1000.);
#3070=VECTOR('',#20373,1000.);
#3071=VECTOR('',#20376,1000.);
#3072=VECTOR('',#20379,1000.);
#3073=VECTOR('',#20382,1000.);
#3074=VECTOR('',#20389,1000.);
#3075=VECTOR('',#20392,1000.);
#3076=VECTOR('',#20395,1000.);
#3077=VECTOR('',#20398,1000.);
#3078=VECTOR('',#20403,1000.);
#3079=VECTOR('',#20406,1000.);
#3080=VECTOR('',#20409,1000.);
#3081=VECTOR('',#20412,1000.);
#3082=VECTOR('',#20415,1000.);
#3083=VECTOR('',#20416,1000.);
#3084=VECTOR('',#20419,1000.);
#3085=VECTOR('',#20422,1000.);
#3086=VECTOR('',#20425,1000.);
#3087=VECTOR('',#20428,1000.);
#3088=VECTOR('',#20431,1000.);
#3089=VECTOR('',#20434,1000.);
#3090=VECTOR('',#20441,1000.);
#3091=VECTOR('',#20444,1000.);
#3092=VECTOR('',#20449,1000.);
#3093=VECTOR('',#20452,1000.);
#3094=VECTOR('',#20457,1000.);
#3095=VECTOR('',#20460,1000.);
#3096=VECTOR('',#20465,1000.);
#3097=VECTOR('',#20468,1000.);
#3098=VECTOR('',#20473,1000.);
#3099=VECTOR('',#20476,1000.);
#3100=VECTOR('',#20481,1000.);
#3101=VECTOR('',#20484,1000.);
#3102=VECTOR('',#20489,1000.);
#3103=VECTOR('',#20492,1000.);
#3104=VECTOR('',#20497,1000.);
#3105=VECTOR('',#20500,1000.);
#3106=VECTOR('',#20505,1000.);
#3107=VECTOR('',#20508,1000.);
#3108=VECTOR('',#20517,1000.);
#3109=VECTOR('',#20520,1000.);
#3110=VECTOR('',#20531,5.);
#3111=VECTOR('',#20536,10.);
#3112=VECTOR('',#20539,10.);
#3113=VECTOR('',#20556,1000.);
#3114=VECTOR('',#20559,1000.);
#3115=VECTOR('',#20588,1000.);
#3116=VECTOR('',#20591,1000.);
#3117=VECTOR('',#20602,5.);
#3118=VECTOR('',#20607,10.);
#3119=VECTOR('',#20610,10.);
#3120=VECTOR('',#20631,1000.);
#3121=VECTOR('',#20634,1000.);
#3122=VECTOR('',#20659,1000.);
#3123=VECTOR('',#20660,1000.);
#3124=VECTOR('',#20665,1000.);
#3125=VECTOR('',#20668,1000.);
#3126=VECTOR('',#20673,1000.);
#3127=VECTOR('',#20676,1000.);
#3128=VECTOR('',#20677,1000.);
#3129=VECTOR('',#20678,1000.);
#3130=VECTOR('',#20683,1000.);
#3131=VECTOR('',#20686,1000.);
#3132=VECTOR('',#20691,1000.);
#3133=VECTOR('',#20694,1000.);
#3134=VECTOR('',#20699,1000.);
#3135=VECTOR('',#20702,1000.);
#3136=VECTOR('',#20707,204.);
#3137=VECTOR('',#20708,204.);
#3138=VECTOR('',#20715,200.);
#3139=VECTOR('',#20716,200.);
#3140=VECTOR('',#20723,1000.);
#3141=VECTOR('',#20724,1000.);
#3142=VECTOR('',#20731,1000.);
#3143=VECTOR('',#20736,1000.);
#3144=VECTOR('',#20759,1000.);
#3145=VECTOR('',#20760,1000.);
#3146=VECTOR('',#20763,1000.);
#3147=VECTOR('',#20764,1000.);
#3148=VECTOR('',#20765,1000.);
#3149=VECTOR('',#20766,1000.);
#3150=VECTOR('',#20767,1000.);
#3151=VECTOR('',#20768,1000.);
#3152=VECTOR('',#20771,1000.);
#3153=VECTOR('',#20772,1000.);
#3154=VECTOR('',#20773,1000.);
#3155=VECTOR('',#20776,1000.);
#3156=VECTOR('',#20777,1000.);
#3157=VECTOR('',#20778,1000.);
#3158=VECTOR('',#20781,1000.);
#3159=VECTOR('',#20782,1000.);
#3160=VECTOR('',#20783,1000.);
#3161=VECTOR('',#20784,1000.);
#3162=VECTOR('',#20787,1000.);
#3163=VECTOR('',#20788,1000.);
#3164=VECTOR('',#20789,1000.);
#3165=VECTOR('',#20790,1000.);
#3166=VECTOR('',#20791,1000.);
#3167=VECTOR('',#20794,1000.);
#3168=VECTOR('',#20795,1000.);
#3169=VECTOR('',#20796,1000.);
#3170=VECTOR('',#20799,1000.);
#3171=VECTOR('',#20800,1000.);
#3172=VECTOR('',#20801,1000.);
#3173=VECTOR('',#20804,1000.);
#3174=VECTOR('',#20807,1000.);
#3175=VECTOR('',#20810,1000.);
#3176=VECTOR('',#20813,1000.);
#3177=VECTOR('',#20816,1000.);
#3178=VECTOR('',#20819,1000.);
#3179=VECTOR('',#20822,1000.);
#3180=VECTOR('',#20825,1000.);
#3181=VECTOR('',#20828,1000.);
#3182=VECTOR('',#20831,1000.);
#3183=VECTOR('',#20834,1000.);
#3184=VECTOR('',#20837,1000.);
#3185=VECTOR('',#20838,1000.);
#3186=VECTOR('',#20843,1000.);
#3187=VECTOR('',#20846,1000.);
#3188=VECTOR('',#20849,1000.);
#3189=VECTOR('',#20852,1000.);
#3190=VECTOR('',#20859,1000.);
#3191=VECTOR('',#20862,1000.);
#3192=VECTOR('',#20867,1000.);
#3193=VECTOR('',#20876,1000.);
#3194=VECTOR('',#20881,1000.);
#3195=VECTOR('',#20886,1000.);
#3196=VECTOR('',#20895,1000.);
#3197=VECTOR('',#20896,1000.);
#3198=VECTOR('',#20897,1000.);
#3199=VECTOR('',#20900,1000.);
#3200=VECTOR('',#20901,1000.);
#3201=VECTOR('',#20902,1000.);
#3202=VECTOR('',#20903,1000.);
#3203=VECTOR('',#20904,1000.);
#3204=VECTOR('',#20905,1000.);
#3205=VECTOR('',#20906,1000.);
#3206=VECTOR('',#20907,1000.);
#3207=VECTOR('',#20908,1000.);
#3208=VECTOR('',#20909,1000.);
#3209=VECTOR('',#20910,1000.);
#3210=VECTOR('',#20911,1000.);
#3211=VECTOR('',#20912,1000.);
#3212=VECTOR('',#20913,1000.);
#3213=VECTOR('',#20914,1000.);
#3214=VECTOR('',#20915,1000.);
#3215=VECTOR('',#20916,1000.);
#3216=VECTOR('',#20917,1000.);
#3217=VECTOR('',#20918,1000.);
#3218=VECTOR('',#20919,1000.);
#3219=VECTOR('',#20920,1000.);
#3220=VECTOR('',#20921,1000.);
#3221=VECTOR('',#20922,1000.);
#3222=VECTOR('',#20923,1000.);
#3223=VECTOR('',#20924,1000.);
#3224=VECTOR('',#20925,1000.);
#3225=VECTOR('',#20926,1000.);
#3226=VECTOR('',#20927,1000.);
#3227=VECTOR('',#20928,1000.);
#3228=VECTOR('',#20929,1000.);
#3229=VECTOR('',#20930,1000.);
#3230=VECTOR('',#20931,1000.);
#3231=VECTOR('',#20932,1000.);
#3232=VECTOR('',#20937,1000.);
#3233=VECTOR('',#20938,1000.);
#3234=VECTOR('',#20945,1000.);
#3235=VECTOR('',#20946,1000.);
#3236=VECTOR('',#20953,1000.);
#3237=VECTOR('',#20956,1000.);
#3238=VECTOR('',#20959,1000.);
#3239=VECTOR('',#20960,1000.);
#3240=VECTOR('',#20967,1000.);
#3241=VECTOR('',#20970,1000.);
#3242=VECTOR('',#20971,1000.);
#3243=VECTOR('',#20978,1000.);
#3244=VECTOR('',#20979,1000.);
#3245=VECTOR('',#20986,1000.);
#3246=VECTOR('',#20987,1000.);
#3247=VECTOR('',#20994,1000.);
#3248=VECTOR('',#20995,1000.);
#3249=VECTOR('',#21002,1000.);
#3250=VECTOR('',#21003,1000.);
#3251=VECTOR('',#21010,1000.);
#3252=VECTOR('',#21011,1000.);
#3253=VECTOR('',#21022,1000.);
#3254=VECTOR('',#21025,1000.);
#3255=VECTOR('',#21064,14.);
#3256=VECTOR('',#21071,14.);
#3257=VECTOR('',#21080,15.);
#3258=VECTOR('',#21083,15.);
#3259=VECTOR('',#21100,6.75000000000001);
#3260=VECTOR('',#21107,6.74999999999998);
#3261=VECTOR('',#21114,6.74999999999998);
#3262=VECTOR('',#21121,6.75000000000001);
#3263=VECTOR('',#21126,1000.);
#3264=VECTOR('',#21127,1000.);
#3265=VECTOR('',#21128,1000.);
#3266=VECTOR('',#21129,1000.);
#3267=VECTOR('',#21130,1000.);
#3268=VECTOR('',#21131,1000.);
#3269=VECTOR('',#21132,1000.);
#3270=VECTOR('',#21133,1000.);
#3271=VECTOR('',#21134,1000.);
#3272=VECTOR('',#21135,1000.);
#3273=VECTOR('',#21136,1000.);
#3274=VECTOR('',#21137,1000.);
#3275=VECTOR('',#21140,1000.);
#3276=VECTOR('',#21141,1000.);
#3277=VECTOR('',#21142,1000.);
#3278=VECTOR('',#21143,1000.);
#3279=VECTOR('',#21144,1000.);
#3280=VECTOR('',#21145,1000.);
#3281=VECTOR('',#21146,1000.);
#3282=VECTOR('',#21147,1000.);
#3283=VECTOR('',#21148,1000.);
#3284=VECTOR('',#21149,1000.);
#3285=VECTOR('',#21150,1000.);
#3286=VECTOR('',#21151,1000.);
#3287=VECTOR('',#21154,1000.);
#3288=VECTOR('',#21155,1000.);
#3289=VECTOR('',#21156,1000.);
#3290=VECTOR('',#21159,1000.);
#3291=VECTOR('',#21160,1000.);
#3292=VECTOR('',#21161,1000.);
#3293=VECTOR('',#21164,1000.);
#3294=VECTOR('',#21165,1000.);
#3295=VECTOR('',#21166,1000.);
#3296=VECTOR('',#21169,1000.);
#3297=VECTOR('',#21170,1000.);
#3298=VECTOR('',#21171,1000.);
#3299=VECTOR('',#21174,1000.);
#3300=VECTOR('',#21175,1000.);
#3301=VECTOR('',#21178,1000.);
#3302=VECTOR('',#21179,1000.);
#3303=VECTOR('',#21180,1000.);
#3304=VECTOR('',#21183,1000.);
#3305=VECTOR('',#21184,1000.);
#3306=VECTOR('',#21185,1000.);
#3307=VECTOR('',#21188,1000.);
#3308=VECTOR('',#21189,1000.);
#3309=VECTOR('',#21190,1000.);
#3310=VECTOR('',#21193,1000.);
#3311=VECTOR('',#21194,1000.);
#3312=VECTOR('',#21195,1000.);
#3313=VECTOR('',#21198,1000.);
#3314=VECTOR('',#21199,1000.);
#3315=VECTOR('',#21204,1000.);
#3316=VECTOR('',#21205,1000.);
#3317=VECTOR('',#21206,1000.);
#3318=VECTOR('',#21207,1000.);
#3319=VECTOR('',#21208,1000.);
#3320=VECTOR('',#21209,1000.);
#3321=VECTOR('',#21212,1000.);
#3322=VECTOR('',#21213,1000.);
#3323=VECTOR('',#21216,1000.);
#3324=VECTOR('',#21217,1000.);
#3325=VECTOR('',#21220,1000.);
#3326=VECTOR('',#21221,1000.);
#3327=VECTOR('',#21222,1000.);
#3328=VECTOR('',#21223,1000.);
#3329=VECTOR('',#21224,1000.);
#3330=VECTOR('',#21227,1000.);
#3331=VECTOR('',#21228,1000.);
#3332=VECTOR('',#21229,1000.);
#3333=VECTOR('',#21230,1000.);
#3334=VECTOR('',#21231,1000.);
#3335=VECTOR('',#21234,1000.);
#3336=VECTOR('',#21235,1000.);
#3337=VECTOR('',#21238,1000.);
#3338=VECTOR('',#21243,1000.);
#3339=VECTOR('',#21244,1000.);
#3340=VECTOR('',#21247,1000.);
#3341=VECTOR('',#21248,1000.);
#3342=VECTOR('',#21251,1000.);
#3343=VECTOR('',#21254,1000.);
#3344=VECTOR('',#21259,1000.);
#3345=VECTOR('',#21268,96.161193339026);
#3346=VECTOR('',#21275,2.5);
#3347=VECTOR('',#21282,2.5);
#3348=VECTOR('',#21289,2.5);
#3349=VECTOR('',#21296,2.5);
#3350=VECTOR('',#21303,2.5);
#3351=VECTOR('',#21310,2.5);
#3352=VECTOR('',#21317,2.5);
#3353=VECTOR('',#21324,2.5);
#3354=VECTOR('',#21331,2.50000000000001);
#3355=VECTOR('',#21338,2.5);
#3356=VECTOR('',#21345,2.5);
#3357=VECTOR('',#21352,2.5);
#3358=VECTOR('',#21359,2.5);
#3359=VECTOR('',#21366,2.5);
#3360=VECTOR('',#21373,2.5);
#3361=VECTOR('',#21380,275.);
#3362=VECTOR('',#21391,96.161193339026);
#3363=VECTOR('',#21450,55.);
#3364=VECTOR('',#21455,28.6682517601201);
#3365=VECTOR('',#21458,50.);
#3366=VECTOR('',#21463,32.793965079916);
#3367=VECTOR('',#21466,45.3097394023382);
#3368=VECTOR('',#21477,0.857142857149274);
#3369=VECTOR('',#21482,0.999999999925893);
#3370=VECTOR('',#21489,0.499999999966139);
#3371=VECTOR('',#21496,1000.);
#3372=VECTOR('',#21497,1000.);
#3373=VECTOR('',#21498,1000.);
#3374=VECTOR('',#21499,1000.);
#3375=VECTOR('',#21500,1000.);
#3376=VECTOR('',#21501,1000.);
#3377=VECTOR('',#21504,1000.);
#3378=VECTOR('',#21505,1000.);
#3379=VECTOR('',#21506,1000.);
#3380=VECTOR('',#21509,1000.);
#3381=VECTOR('',#21510,1000.);
#3382=VECTOR('',#21513,1000.);
#3383=VECTOR('',#21514,1000.);
#3384=VECTOR('',#21515,1000.);
#3385=VECTOR('',#21518,1000.);
#3386=VECTOR('',#21519,1000.);
#3387=VECTOR('',#21522,1000.);
#3388=VECTOR('',#21523,1000.);
#3389=VECTOR('',#21526,1000.);
#3390=VECTOR('',#21527,1000.);
#3391=VECTOR('',#21530,1000.);
#3392=VECTOR('',#21533,10.);
#3393=VECTOR('',#21534,10.);
#3394=VECTOR('',#21535,10.);
#3395=VECTOR('',#21550,6.75000000000001);
#3396=VECTOR('',#21557,6.75);
#3397=VECTOR('',#21564,6.75000000000001);
#3398=VECTOR('',#21571,6.75);
#3399=VECTOR('',#21580,7.00000000000001);
#3400=VECTOR('',#21611,7.);
#3401=VECTOR('',#21618,7.);
#3402=VECTOR('',#21633,7.);
#3403=VECTOR('',#21644,80.);
#3404=VECTOR('',#21651,40.);
#3405=VECTOR('',#21656,1000.);
#3406=VECTOR('',#21657,1000.);
#3407=VECTOR('',#21660,1000.);
#3408=VECTOR('',#21661,1000.);
#3409=VECTOR('',#21666,1000.);
#3410=VECTOR('',#21669,1000.);
#3411=VECTOR('',#21672,1000.);
#3412=VECTOR('',#21675,1000.);
#3413=VECTOR('',#21678,1000.);
#3414=VECTOR('',#21679,1000.);
#3415=VECTOR('',#21686,1000.);
#3416=VECTOR('',#21689,1000.);
#3417=VECTOR('',#21694,4.5);
#3418=VECTOR('',#21701,4.5);
#3419=VECTOR('',#21708,4.5);
#3420=VECTOR('',#21715,4.5);
#3421=VECTOR('',#21722,20.);
#3422=VECTOR('',#21729,1000.);
#3423=VECTOR('',#21730,1000.);
#3424=VECTOR('',#21735,1000.);
#3425=VECTOR('',#21736,1000.);
#3426=VECTOR('',#21741,1000.);
#3427=VECTOR('',#21744,1000.);
#3428=VECTOR('',#21757,76.5);
#3429=VECTOR('',#21772,7.00000000000001);
#3430=VECTOR('',#21783,1000.);
#3431=VECTOR('',#21786,1000.);
#3432=VECTOR('',#21791,1000.);
#3433=VECTOR('',#21794,1000.);
#3434=VECTOR('',#21795,1000.);
#3435=VECTOR('',#21798,1000.);
#3436=VECTOR('',#21801,6.99999999990287);
#3437=VECTOR('',#21808,4.);
#3438=VECTOR('',#21815,4.);
#3439=VECTOR('',#21822,4.);
#3440=VECTOR('',#21829,4.);
#3441=VECTOR('',#21836,17.4625);
#3442=VECTOR('',#21839,1000.);
#3443=VECTOR('',#21842,17.4625);
#3444=VECTOR('',#21847,1000.);
#3445=VECTOR('',#21854,7.99999999999999);
#3446=VECTOR('',#21861,8.00000000000001);
#3447=VECTOR('',#21866,17.4625);
#3448=VECTOR('',#21873,7.00000000000001);
#3449=VECTOR('',#21880,7.00000000000001);
#3450=VECTOR('',#21887,3.);
#3451=VECTOR('',#21894,3.00000000000307);
#3452=VECTOR('',#21901,3.0000000000021);
#3453=VECTOR('',#21908,2.99999999999927);
#3454=VECTOR('',#21915,1000.);
#3455=VECTOR('',#21918,1000.);
#3456=VECTOR('',#21921,6.7500000000354);
#3457=VECTOR('',#21930,1000.);
#3458=VECTOR('',#21933,1000.);
#3459=VECTOR('',#21940,6.75000000001091);
#3460=VECTOR('',#21947,5.5);
#3461=VECTOR('',#21954,1000.);
#3462=VECTOR('',#21957,1000.);
#3463=VECTOR('',#21966,8.80000000000425);
#3464=VECTOR('',#21973,8.80000000000425);
#3465=VECTOR('',#21978,6.34999999994079);
#3466=VECTOR('',#21985,5.5);
#3467=VECTOR('',#21994,1000.);
#3468=VECTOR('',#21997,1000.);
#3469=VECTOR('',#22000,5.4999999998131);
#3470=VECTOR('',#22005,10.);
#3471=VECTOR('',#22006,10.);
#3472=VECTOR('',#22007,10.);
#3473=VECTOR('',#22008,10.);
#3474=VECTOR('',#22011,10.);
#3475=VECTOR('',#22012,10.);
#3476=VECTOR('',#22015,10.);
#3477=VECTOR('',#22016,10.);
#3478=VECTOR('',#22023,1000.);
#3479=VECTOR('',#22024,1000.);
#3480=VECTOR('',#22025,1000.);
#3481=VECTOR('',#22026,1000.);
#3482=VECTOR('',#22027,1000.);
#3483=VECTOR('',#22028,1000.);
#3484=VECTOR('',#22031,1000.);
#3485=VECTOR('',#22032,1000.);
#3486=VECTOR('',#22033,1000.);
#3487=VECTOR('',#22034,1000.);
#3488=VECTOR('',#22035,1000.);
#3489=VECTOR('',#22036,1000.);
#3490=VECTOR('',#22039,1000.);
#3491=VECTOR('',#22040,1000.);
#3492=VECTOR('',#22041,1000.);
#3493=VECTOR('',#22042,1000.);
#3494=VECTOR('',#22043,1000.);
#3495=VECTOR('',#22044,1000.);
#3496=VECTOR('',#22047,1000.);
#3497=VECTOR('',#22048,1000.);
#3498=VECTOR('',#22049,1000.);
#3499=VECTOR('',#22050,1000.);
#3500=VECTOR('',#22051,1000.);
#3501=VECTOR('',#22052,1000.);
#3502=VECTOR('',#22057,1000.);
#3503=VECTOR('',#22064,1000.);
#3504=VECTOR('',#22069,1000.);
#3505=VECTOR('',#22076,1000.);
#3506=VECTOR('',#22083,1000.);
#3507=VECTOR('',#22084,1000.);
#3508=VECTOR('',#22085,1000.);
#3509=VECTOR('',#22086,1000.);
#3510=VECTOR('',#22087,1000.);
#3511=VECTOR('',#22088,1000.);
#3512=VECTOR('',#22091,1000.);
#3513=VECTOR('',#22092,1000.);
#3514=VECTOR('',#22093,1000.);
#3515=VECTOR('',#22094,1000.);
#3516=VECTOR('',#22095,1000.);
#3517=VECTOR('',#22096,1000.);
#3518=VECTOR('',#22099,1000.);
#3519=VECTOR('',#22100,1000.);
#3520=VECTOR('',#22101,1000.);
#3521=VECTOR('',#22104,1000.);
#3522=VECTOR('',#22105,1000.);
#3523=VECTOR('',#22108,1000.);
#3524=VECTOR('',#22109,1000.);
#3525=VECTOR('',#22112,1000.);
#3526=VECTOR('',#22113,1000.);
#3527=VECTOR('',#22116,1000.);
#3528=VECTOR('',#22117,1000.);
#3529=VECTOR('',#22120,1000.);
#3530=VECTOR('',#22123,1000.);
#3531=VECTOR('',#22124,1000.);
#3532=VECTOR('',#22125,1000.);
#3533=VECTOR('',#22126,1000.);
#3534=VECTOR('',#22131,1000.);
#3535=VECTOR('',#22138,1000.);
#3536=VECTOR('',#22139,1000.);
#3537=VECTOR('',#22140,1000.);
#3538=VECTOR('',#22145,1000.);
#3539=VECTOR('',#22146,1000.);
#3540=VECTOR('',#22147,1000.);
#3541=VECTOR('',#22150,1000.);
#3542=VECTOR('',#22151,1000.);
#3543=VECTOR('',#22154,1000.);
#3544=VECTOR('',#22155,1000.);
#3545=VECTOR('',#22158,1000.);
#3546=VECTOR('',#22159,1000.);
#3547=VECTOR('',#22162,1000.);
#3548=VECTOR('',#22163,1000.);
#3549=VECTOR('',#22166,1000.);
#3550=VECTOR('',#22169,1000.);
#3551=VECTOR('',#22170,1000.);
#3552=VECTOR('',#22171,1000.);
#3553=VECTOR('',#22172,1000.);
#3554=VECTOR('',#22177,1000.);
#3555=VECTOR('',#22184,1000.);
#3556=VECTOR('',#22185,1000.);
#3557=VECTOR('',#22186,1000.);
#3558=VECTOR('',#22191,1000.);
#3559=VECTOR('',#22192,1000.);
#3560=VECTOR('',#22193,1000.);
#3561=VECTOR('',#22196,1000.);
#3562=VECTOR('',#22197,1000.);
#3563=VECTOR('',#22200,1000.);
#3564=VECTOR('',#22201,1000.);
#3565=VECTOR('',#22204,1000.);
#3566=VECTOR('',#22205,1000.);
#3567=VECTOR('',#22208,1000.);
#3568=VECTOR('',#22209,1000.);
#3569=VECTOR('',#22212,1000.);
#3570=VECTOR('',#22215,1000.);
#3571=VECTOR('',#22216,1000.);
#3572=VECTOR('',#22217,1000.);
#3573=VECTOR('',#22218,1000.);
#3574=VECTOR('',#22223,1000.);
#3575=VECTOR('',#22230,1000.);
#3576=VECTOR('',#22231,1000.);
#3577=VECTOR('',#22232,1000.);
#3578=VECTOR('',#22237,1000.);
#3579=VECTOR('',#22238,1000.);
#3580=VECTOR('',#22239,1000.);
#3581=VECTOR('',#22242,1000.);
#3582=VECTOR('',#22243,1000.);
#3583=VECTOR('',#22244,1000.);
#3584=VECTOR('',#22247,1000.);
#3585=VECTOR('',#22248,1000.);
#3586=VECTOR('',#22249,1000.);
#3587=VECTOR('',#22252,1000.);
#3588=VECTOR('',#22253,1000.);
#3589=VECTOR('',#22256,1000.);
#3590=VECTOR('',#22257,1000.);
#3591=VECTOR('',#22260,1000.);
#3592=VECTOR('',#22261,1000.);
#3593=VECTOR('',#22264,1000.);
#3594=VECTOR('',#22265,1000.);
#3595=VECTOR('',#22268,1000.);
#3596=VECTOR('',#22271,1000.);
#3597=VECTOR('',#22272,1000.);
#3598=VECTOR('',#22273,1000.);
#3599=VECTOR('',#22278,1000.);
#3600=VECTOR('',#22283,1000.);
#3601=VECTOR('',#22284,1000.);
#3602=VECTOR('',#22289,1000.);
#3603=VECTOR('',#22290,1000.);
#3604=VECTOR('',#22295,1000.);
#3605=VECTOR('',#22296,1000.);
#3606=VECTOR('',#22299,1000.);
#3607=VECTOR('',#22304,1000.);
#3608=VECTOR('',#22309,1000.);
#3609=VECTOR('',#22314,1000.);
#3610=VECTOR('',#22315,1000.);
#3611=VECTOR('',#22318,1000.);
#3612=VECTOR('',#22323,1000.);
#3613=VECTOR('',#22328,1000.);
#3614=VECTOR('',#22333,1000.);
#3615=VECTOR('',#22334,1000.);
#3616=VECTOR('',#22341,1000.);
#3617=VECTOR('',#22346,1000.);
#3618=VECTOR('',#22347,1000.);
#3619=VECTOR('',#22350,1000.);
#3620=VECTOR('',#22359,1000.);
#3621=VECTOR('',#22360,1000.);
#3622=VECTOR('',#22365,1000.);
#3623=VECTOR('',#22370,1000.);
#3624=VECTOR('',#22375,1000.);
#3625=VECTOR('',#22380,1000.);
#3626=VECTOR('',#22389,1000.);
#3627=VECTOR('',#22390,1000.);
#3628=VECTOR('',#22395,1000.);
#3629=VECTOR('',#22400,1000.);
#3630=VECTOR('',#22405,1000.);
#3631=VECTOR('',#22410,1000.);
#3632=VECTOR('',#22419,1000.);
#3633=VECTOR('',#22422,1000.);
#3634=VECTOR('',#22427,1000.);
#3635=VECTOR('',#22428,1000.);
#3636=VECTOR('',#22431,1000.);
#3637=VECTOR('',#22434,1000.);
#3638=VECTOR('',#22437,1000.);
#3639=VECTOR('',#22440,1000.);
#3640=VECTOR('',#22443,1000.);
#3641=VECTOR('',#22446,1000.);
#3642=VECTOR('',#22449,1000.);
#3643=VECTOR('',#22452,1000.);
#3644=VECTOR('',#22455,1000.);
#3645=VECTOR('',#22456,1000.);
#3646=VECTOR('',#22461,1000.);
#3647=VECTOR('',#22464,1000.);
#3648=VECTOR('',#22467,1000.);
#3649=VECTOR('',#22468,1000.);
#3650=VECTOR('',#22473,1000.);
#3651=VECTOR('',#22476,1000.);
#3652=VECTOR('',#22479,1000.);
#3653=VECTOR('',#22480,1000.);
#3654=VECTOR('',#22485,1000.);
#3655=VECTOR('',#22488,1000.);
#3656=VECTOR('',#22491,1000.);
#3657=VECTOR('',#22492,1000.);
#3658=VECTOR('',#22497,1000.);
#3659=VECTOR('',#22500,1000.);
#3660=VECTOR('',#22527,1000.);
#3661=VECTOR('',#22528,1000.);
#3662=VECTOR('',#22531,1000.);
#3663=VECTOR('',#22532,1000.);
#3664=VECTOR('',#22537,1000.);
#3665=VECTOR('',#22540,1000.);
#3666=VECTOR('',#22541,1000.);
#3667=VECTOR('',#22546,1000.);
#3668=VECTOR('',#22549,1000.);
#3669=VECTOR('',#22550,1000.);
#3670=VECTOR('',#22555,1000.);
#3671=VECTOR('',#22558,1000.);
#3672=VECTOR('',#22559,10.);
#3673=VECTOR('',#22560,10.);
#3674=VECTOR('',#22561,10.);
#3675=VECTOR('',#22562,10.);
#3676=VECTOR('',#22567,10.);
#3677=VECTOR('',#22568,10.);
#3678=VECTOR('',#22573,10.);
#3679=VECTOR('',#22574,10.);
#3680=VECTOR('',#22579,10.);
#3681=VECTOR('',#22580,10.);
#3682=VECTOR('',#22591,10.);
#3683=VECTOR('',#22594,10.);
#3684=VECTOR('',#22595,10.);
#3685=VECTOR('',#22598,10.);
#3686=VECTOR('',#22599,10.);
#3687=VECTOR('',#22606,1000.);
#3688=VECTOR('',#22607,1000.);
#3689=VECTOR('',#22612,1000.);
#3690=VECTOR('',#22613,1000.);
#3691=VECTOR('',#22618,1000.);
#3692=VECTOR('',#22619,1000.);
#3693=VECTOR('',#22624,10.);
#3694=VECTOR('',#22625,10.);
#3695=VECTOR('',#22638,10.);
#3696=VECTOR('',#22639,10.);
#3697=VECTOR('',#22644,10.);
#3698=VECTOR('',#22645,10.);
#3699=VECTOR('',#22650,10.);
#3700=VECTOR('',#22651,10.);
#3701=VECTOR('',#22654,1000.);
#3702=VECTOR('',#22657,1000.);
#3703=VECTOR('',#22660,1000.);
#3704=VECTOR('',#22663,1000.);
#3705=VECTOR('',#22670,1000.);
#3706=VECTOR('',#22671,1000.);
#3707=VECTOR('',#22676,1000.);
#3708=VECTOR('',#22681,1000.);
#3709=VECTOR('',#22684,1000.);
#3710=VECTOR('',#22691,1000.);
#3711=VECTOR('',#22696,1000.);
#3712=VECTOR('',#22705,1000.);
#3713=VECTOR('',#22710,1000.);
#3714=VECTOR('',#22717,1000.);
#3715=VECTOR('',#22724,1000.);
#3716=VECTOR('',#22729,1000.);
#3717=VECTOR('',#22734,1000.);
#3718=VECTOR('',#22741,1000.);
#3719=VECTOR('',#22742,1000.);
#3720=VECTOR('',#22743,1000.);
#3721=VECTOR('',#22746,1000.);
#3722=VECTOR('',#22747,1000.);
#3723=VECTOR('',#22748,1000.);
#3724=VECTOR('',#22755,1000.);
#3725=VECTOR('',#22756,1000.);
#3726=VECTOR('',#22757,1000.);
#3727=VECTOR('',#22766,1000.);
#3728=VECTOR('',#22769,1000.);
#3729=VECTOR('',#22774,1000.);
#3730=VECTOR('',#22775,1000.);
#3731=VECTOR('',#22780,1000.);
#3732=VECTOR('',#22783,1000.);
#3733=VECTOR('',#22786,1000.);
#3734=VECTOR('',#22791,1000.);
#3735=VECTOR('',#22794,1000.);
#3736=VECTOR('',#22803,1000.);
#3737=VECTOR('',#22808,1000.);
#3738=VECTOR('',#22837,1000.);
#3739=VECTOR('',#22838,1000.);
#3740=VECTOR('',#22839,1000.);
#3741=VECTOR('',#22840,1000.);
#3742=VECTOR('',#22841,1000.);
#3743=VECTOR('',#22842,1000.);
#3744=VECTOR('',#22845,1000.);
#3745=VECTOR('',#22846,1000.);
#3746=VECTOR('',#22847,1000.);
#3747=VECTOR('',#22848,1000.);
#3748=VECTOR('',#22849,1000.);
#3749=VECTOR('',#22850,1000.);
#3750=VECTOR('',#22853,1000.);
#3751=VECTOR('',#22856,1000.);
#3752=VECTOR('',#22859,1000.);
#3753=VECTOR('',#22862,1000.);
#3754=VECTOR('',#22867,1000.);
#3755=VECTOR('',#22870,1000.);
#3756=VECTOR('',#22871,1000.);
#3757=VECTOR('',#22874,1000.);
#3758=VECTOR('',#22875,1000.);
#3759=VECTOR('',#22878,1000.);
#3760=VECTOR('',#22883,1000.);
#3761=VECTOR('',#22886,1000.);
#3762=VECTOR('',#22895,1000.);
#3763=VECTOR('',#22896,1000.);
#3764=VECTOR('',#22899,1000.);
#3765=VECTOR('',#22900,1000.);
#3766=VECTOR('',#22903,1000.);
#3767=VECTOR('',#22914,1000.);
#3768=VECTOR('',#22915,1000.);
#3769=VECTOR('',#22918,1000.);
#3770=VECTOR('',#22919,1000.);
#3771=VECTOR('',#22922,1000.);
#3772=VECTOR('',#22927,1000.);
#3773=VECTOR('',#22930,1000.);
#3774=VECTOR('',#22939,1000.);
#3775=VECTOR('',#22940,1000.);
#3776=VECTOR('',#22943,1000.);
#3777=VECTOR('',#22944,1000.);
#3778=VECTOR('',#22947,1000.);
#3779=VECTOR('',#22952,1000.);
#3780=VECTOR('',#22959,1000.);
#3781=VECTOR('',#22960,1000.);
#3782=VECTOR('',#22961,1000.);
#3783=VECTOR('',#22964,1000.);
#3784=VECTOR('',#22965,1000.);
#3785=VECTOR('',#22968,1000.);
#3786=VECTOR('',#22969,1000.);
#3787=VECTOR('',#22972,1000.);
#3788=VECTOR('',#22973,1000.);
#3789=VECTOR('',#22976,1000.);
#3790=VECTOR('',#22977,1000.);
#3791=VECTOR('',#22980,1000.);
#3792=VECTOR('',#22983,1000.);
#3793=VECTOR('',#22984,1000.);
#3794=VECTOR('',#22985,1000.);
#3795=VECTOR('',#22988,1000.);
#3796=VECTOR('',#22989,1000.);
#3797=VECTOR('',#22992,1000.);
#3798=VECTOR('',#22993,1000.);
#3799=VECTOR('',#22996,1000.);
#3800=VECTOR('',#22997,1000.);
#3801=VECTOR('',#23000,1000.);
#3802=VECTOR('',#23001,1000.);
#3803=VECTOR('',#23004,1000.);
#3804=VECTOR('',#23009,1000.);
#3805=VECTOR('',#23012,1000.);
#3806=VECTOR('',#23017,1000.);
#3807=VECTOR('',#23020,1000.);
#3808=VECTOR('',#23023,1000.);
#3809=VECTOR('',#23024,1000.);
#3810=VECTOR('',#23025,1000.);
#3811=VECTOR('',#23026,1000.);
#3812=VECTOR('',#23029,1000.);
#3813=VECTOR('',#23032,1000.);
#3814=VECTOR('',#23033,1000.);
#3815=VECTOR('',#23034,1000.);
#3816=VECTOR('',#23037,1000.);
#3817=VECTOR('',#23038,1000.);
#3818=VECTOR('',#23045,1000.);
#3819=VECTOR('',#23048,1000.);
#3820=VECTOR('',#23053,1000.);
#3821=VECTOR('',#23056,1000.);
#3822=VECTOR('',#23061,1000.);
#3823=VECTOR('',#23064,1000.);
#3824=VECTOR('',#23067,1000.);
#3825=VECTOR('',#23068,1000.);
#3826=VECTOR('',#23069,1000.);
#3827=VECTOR('',#23070,1000.);
#3828=VECTOR('',#23071,1000.);
#3829=VECTOR('',#23072,1000.);
#3830=VECTOR('',#23075,1000.);
#3831=VECTOR('',#23076,1000.);
#3832=VECTOR('',#23081,1000.);
#3833=VECTOR('',#23082,1000.);
#3834=VECTOR('',#23089,1000.);
#3835=VECTOR('',#23090,1000.);
#3836=VECTOR('',#23091,1000.);
#3837=VECTOR('',#23094,1000.);
#3838=VECTOR('',#23095,1000.);
#3839=VECTOR('',#23096,1000.);
#3840=VECTOR('',#23099,1000.);
#3841=VECTOR('',#23102,1000.);
#3842=VECTOR('',#23103,1000.);
#3843=VECTOR('',#23104,1000.);
#3844=VECTOR('',#23107,1000.);
#3845=VECTOR('',#23110,1000.);
#3846=VECTOR('',#23113,1000.);
#3847=VECTOR('',#23118,1000.);
#3848=VECTOR('',#23119,1000.);
#3849=VECTOR('',#23120,1000.);
#3850=VECTOR('',#23121,1000.);
#3851=VECTOR('',#23124,1000.);
#3852=VECTOR('',#23125,1000.);
#3853=VECTOR('',#23128,1000.);
#3854=VECTOR('',#23131,1000.);
#3855=VECTOR('',#23132,1000.);
#3856=VECTOR('',#23135,1000.);
#3857=VECTOR('',#23136,1000.);
#3858=VECTOR('',#23139,1000.);
#3859=VECTOR('',#23140,1000.);
#3860=VECTOR('',#23141,1000.);
#3861=VECTOR('',#23142,1000.);
#3862=VECTOR('',#23145,1000.);
#3863=VECTOR('',#23146,1000.);
#3864=VECTOR('',#23147,1000.);
#3865=VECTOR('',#23150,1000.);
#3866=VECTOR('',#23151,1000.);
#3867=VECTOR('',#23152,1000.);
#3868=VECTOR('',#23155,1000.);
#3869=VECTOR('',#23158,1000.);
#3870=VECTOR('',#23161,1000.);
#3871=VECTOR('',#23164,1000.);
#3872=VECTOR('',#23169,1000.);
#3873=VECTOR('',#23170,1000.);
#3874=VECTOR('',#23171,1000.);
#3875=VECTOR('',#23174,1000.);
#3876=VECTOR('',#23175,1000.);
#3877=VECTOR('',#23178,1000.);
#3878=VECTOR('',#23179,1000.);
#3879=VECTOR('',#23180,1000.);
#3880=VECTOR('',#23183,1000.);
#3881=VECTOR('',#23186,1000.);
#3882=VECTOR('',#23187,1000.);
#3883=VECTOR('',#23188,1000.);
#3884=VECTOR('',#23191,1000.);
#3885=VECTOR('',#23194,1000.);
#3886=VECTOR('',#23197,1000.);
#3887=VECTOR('',#23202,1000.);
#3888=VECTOR('',#23203,1000.);
#3889=VECTOR('',#23204,1000.);
#3890=VECTOR('',#23207,1000.);
#3891=VECTOR('',#23208,1000.);
#3892=VECTOR('',#23211,1000.);
#3893=VECTOR('',#23214,1000.);
#3894=VECTOR('',#23219,1000.);
#3895=VECTOR('',#23220,1000.);
#3896=VECTOR('',#23221,1000.);
#3897=VECTOR('',#23224,1000.);
#3898=VECTOR('',#23225,1000.);
#3899=VECTOR('',#23228,1000.);
#3900=VECTOR('',#23231,1000.);
#3901=VECTOR('',#23232,1000.);
#3902=VECTOR('',#23233,1000.);
#3903=VECTOR('',#23236,1000.);
#3904=VECTOR('',#23239,1000.);
#3905=VECTOR('',#23240,1000.);
#3906=VECTOR('',#23241,1000.);
#3907=VECTOR('',#23242,1000.);
#3908=VECTOR('',#23243,1000.);
#3909=VECTOR('',#23244,1000.);
#3910=VECTOR('',#23247,1000.);
#3911=VECTOR('',#23248,1000.);
#3912=VECTOR('',#23249,1000.);
#3913=VECTOR('',#23250,1000.);
#3914=VECTOR('',#23255,1000.);
#3915=VECTOR('',#23256,1000.);
#3916=VECTOR('',#23257,1000.);
#3917=VECTOR('',#23258,1000.);
#3918=VECTOR('',#23263,1000.);
#3919=VECTOR('',#23266,1000.);
#3920=VECTOR('',#23269,1000.);
#3921=VECTOR('',#23270,1000.);
#3922=VECTOR('',#23271,1000.);
#3923=VECTOR('',#23274,1000.);
#3924=VECTOR('',#23279,1000.);
#3925=VECTOR('',#23280,1000.);
#3926=VECTOR('',#23283,1000.);
#3927=VECTOR('',#23284,1000.);
#3928=VECTOR('',#23287,1000.);
#3929=VECTOR('',#23288,1000.);
#3930=VECTOR('',#23291,1000.);
#3931=VECTOR('',#23296,1000.);
#3932=VECTOR('',#23297,1000.);
#3933=VECTOR('',#23298,1000.);
#3934=VECTOR('',#23301,1000.);
#3935=VECTOR('',#23302,1000.);
#3936=VECTOR('',#23303,1000.);
#3937=VECTOR('',#23308,1000.);
#3938=VECTOR('',#23311,1000.);
#3939=VECTOR('',#23314,1000.);
#3940=VECTOR('',#23315,1000.);
#3941=VECTOR('',#23316,1000.);
#3942=VECTOR('',#23319,1000.);
#3943=VECTOR('',#23324,1000.);
#3944=VECTOR('',#23325,1000.);
#3945=VECTOR('',#23328,1000.);
#3946=VECTOR('',#23329,1000.);
#3947=VECTOR('',#23332,1000.);
#3948=VECTOR('',#23333,1000.);
#3949=VECTOR('',#23336,1000.);
#3950=VECTOR('',#23341,1000.);
#3951=VECTOR('',#23342,1000.);
#3952=VECTOR('',#23343,1000.);
#3953=VECTOR('',#23346,1000.);
#3954=VECTOR('',#23347,1000.);
#3955=VECTOR('',#23348,1000.);
#3956=VECTOR('',#23353,1000.);
#3957=VECTOR('',#23356,1000.);
#3958=VECTOR('',#23359,1000.);
#3959=VECTOR('',#23360,1000.);
#3960=VECTOR('',#23361,1000.);
#3961=VECTOR('',#23364,1000.);
#3962=VECTOR('',#23369,1000.);
#3963=VECTOR('',#23370,1000.);
#3964=VECTOR('',#23373,1000.);
#3965=VECTOR('',#23374,1000.);
#3966=VECTOR('',#23377,1000.);
#3967=VECTOR('',#23378,1000.);
#3968=VECTOR('',#23381,1000.);
#3969=VECTOR('',#23386,1000.);
#3970=VECTOR('',#23387,1000.);
#3971=VECTOR('',#23388,1000.);
#3972=VECTOR('',#23391,1000.);
#3973=VECTOR('',#23392,1000.);
#3974=VECTOR('',#23393,1000.);
#3975=VECTOR('',#23398,1000.);
#3976=VECTOR('',#23401,1000.);
#3977=VECTOR('',#23404,1000.);
#3978=VECTOR('',#23405,1000.);
#3979=VECTOR('',#23406,1000.);
#3980=VECTOR('',#23409,1000.);
#3981=VECTOR('',#23414,1000.);
#3982=VECTOR('',#23415,1000.);
#3983=VECTOR('',#23418,1000.);
#3984=VECTOR('',#23419,1000.);
#3985=VECTOR('',#23422,1000.);
#3986=VECTOR('',#23423,1000.);
#3987=VECTOR('',#23426,1000.);
#3988=VECTOR('',#23431,1000.);
#3989=VECTOR('',#23432,1000.);
#3990=VECTOR('',#23435,1000.);
#3991=VECTOR('',#23436,1000.);
#3992=VECTOR('',#23437,1000.);
#3993=VECTOR('',#23440,1000.);
#3994=VECTOR('',#23441,1000.);
#3995=VECTOR('',#23444,1000.);
#3996=VECTOR('',#23445,1000.);
#3997=VECTOR('',#23448,1000.);
#3998=VECTOR('',#23449,1000.);
#3999=VECTOR('',#23452,1000.);
#4000=VECTOR('',#23453,1000.);
#4001=VECTOR('',#23456,1000.);
#4002=VECTOR('',#23463,1000.);
#4003=VECTOR('',#23464,1000.);
#4004=VECTOR('',#23467,1000.);
#4005=VECTOR('',#23470,1000.);
#4006=VECTOR('',#23483,1000.);
#4007=VECTOR('',#23484,1000.);
#4008=VECTOR('',#23485,1000.);
#4009=VECTOR('',#23488,1000.);
#4010=VECTOR('',#23491,1000.);
#4011=VECTOR('',#23494,1000.);
#4012=VECTOR('',#23499,1000.);
#4013=VECTOR('',#23500,1000.);
#4014=VECTOR('',#23503,1000.);
#4015=VECTOR('',#23508,1000.);
#4016=VECTOR('',#23509,1000.);
#4017=VECTOR('',#23512,1000.);
#4018=VECTOR('',#23515,1000.);
#4019=VECTOR('',#23518,1000.);
#4020=VECTOR('',#23521,1000.);
#4021=VECTOR('',#23524,1000.);
#4022=VECTOR('',#23527,1000.);
#4023=VECTOR('',#23530,1000.);
#4024=VECTOR('',#23533,1000.);
#4025=VECTOR('',#23536,1000.);
#4026=VECTOR('',#23539,1000.);
#4027=VECTOR('',#23540,1000.);
#4028=VECTOR('',#23543,1000.);
#4029=VECTOR('',#23548,1000.);
#4030=VECTOR('',#23549,1000.);
#4031=VECTOR('',#23552,1000.);
#4032=VECTOR('',#23555,1000.);
#4033=VECTOR('',#23558,1000.);
#4034=VECTOR('',#23563,1000.);
#4035=VECTOR('',#23564,1000.);
#4036=VECTOR('',#23573,1000.);
#4037=VECTOR('',#23574,1000.);
#4038=VECTOR('',#23575,1000.);
#4039=VECTOR('',#23576,1000.);
#4040=VECTOR('',#23577,1000.);
#4041=VECTOR('',#23578,1000.);
#4042=VECTOR('',#23581,1000.);
#4043=VECTOR('',#23582,1000.);
#4044=VECTOR('',#23585,1000.);
#4045=VECTOR('',#23588,1000.);
#4046=VECTOR('',#23591,1000.);
#4047=VECTOR('',#23594,1000.);
#4048=VECTOR('',#23597,1000.);
#4049=VECTOR('',#23602,1000.);
#4050=VECTOR('',#23605,1000.);
#4051=VECTOR('',#23608,1000.);
#4052=VECTOR('',#23611,1000.);
#4053=VECTOR('',#23614,1000.);
#4054=VECTOR('',#23617,1000.);
#4055=VECTOR('',#23620,1000.);
#4056=VECTOR('',#23625,1000.);
#4057=VECTOR('',#23626,1000.);
#4058=VECTOR('',#23627,1000.);
#4059=VECTOR('',#23628,1000.);
#4060=VECTOR('',#23629,1000.);
#4061=VECTOR('',#23630,1000.);
#4062=VECTOR('',#23631,1000.);
#4063=VECTOR('',#23632,1000.);
#4064=VECTOR('',#23643,1000.);
#4065=VECTOR('',#23648,1000.);
#4066=VECTOR('',#23649,1000.);
#4067=VECTOR('',#23650,1000.);
#4068=VECTOR('',#23651,1000.);
#4069=VECTOR('',#23652,1000.);
#4070=VECTOR('',#23653,1000.);
#4071=VECTOR('',#23654,1000.);
#4072=VECTOR('',#23657,1000.);
#4073=VECTOR('',#23658,1000.);
#4074=VECTOR('',#23659,1000.);
#4075=VECTOR('',#23660,1000.);
#4076=VECTOR('',#23661,1000.);
#4077=VECTOR('',#23662,1000.);
#4078=VECTOR('',#23667,1000.);
#4079=VECTOR('',#23668,1000.);
#4080=VECTOR('',#23669,1000.);
#4081=VECTOR('',#23672,1000.);
#4082=VECTOR('',#23673,1000.);
#4083=VECTOR('',#23676,1000.);
#4084=VECTOR('',#23677,1000.);
#4085=VECTOR('',#23680,1000.);
#4086=VECTOR('',#23681,1000.);
#4087=VECTOR('',#23684,1000.);
#4088=VECTOR('',#23685,1000.);
#4089=VECTOR('',#23688,1000.);
#4090=VECTOR('',#23691,1000.);
#4091=VECTOR('',#23694,1000.);
#4092=VECTOR('',#23719,1000.);
#4093=VECTOR('',#23720,1000.);
#4094=VECTOR('',#23723,1000.);
#4095=VECTOR('',#23724,1000.);
#4096=VECTOR('',#23725,1000.);
#4097=VECTOR('',#23726,1000.);
#4098=VECTOR('',#23727,1000.);
#4099=VECTOR('',#23728,1000.);
#4100=VECTOR('',#23731,1000.);
#4101=VECTOR('',#23732,1000.);
#4102=VECTOR('',#23733,1000.);
#4103=VECTOR('',#23734,1000.);
#4104=VECTOR('',#23735,1000.);
#4105=VECTOR('',#23736,1000.);
#4106=VECTOR('',#23739,1000.);
#4107=VECTOR('',#23740,1000.);
#4108=VECTOR('',#23741,1000.);
#4109=VECTOR('',#23742,1000.);
#4110=VECTOR('',#23743,1000.);
#4111=VECTOR('',#23744,1000.);
#4112=VECTOR('',#23749,1000.);
#4113=VECTOR('',#23752,1000.);
#4114=VECTOR('',#23753,1000.);
#4115=VECTOR('',#23762,1000.);
#4116=VECTOR('',#23765,1000.);
#4117=VECTOR('',#23766,1000.);
#4118=VECTOR('',#23781,1000.);
#4119=VECTOR('',#23784,1000.);
#4120=VECTOR('',#23785,1000.);
#4121=VECTOR('',#23794,1000.);
#4122=VECTOR('',#23797,1000.);
#4123=VECTOR('',#23798,1000.);
#4124=VECTOR('',#23805,1000.);
#4125=VECTOR('',#23806,1000.);
#4126=VECTOR('',#23807,1000.);
#4127=VECTOR('',#23810,1000.);
#4128=VECTOR('',#23811,1000.);
#4129=VECTOR('',#23814,1000.);
#4130=VECTOR('',#23815,1000.);
#4131=VECTOR('',#23818,1000.);
#4132=VECTOR('',#23819,1000.);
#4133=VECTOR('',#23822,1000.);
#4134=VECTOR('',#23823,1000.);
#4135=VECTOR('',#23826,1000.);
#4136=VECTOR('',#23831,1000.);
#4137=VECTOR('',#23832,1000.);
#4138=VECTOR('',#23839,1000.);
#4139=VECTOR('',#23842,1000.);
#4140=VECTOR('',#23845,1000.);
#4141=VECTOR('',#23854,1000.);
#4142=VECTOR('',#23855,1000.);
#4143=VECTOR('',#23856,1000.);
#4144=VECTOR('',#23857,1000.);
#4145=VECTOR('',#23858,1000.);
#4146=VECTOR('',#23859,1000.);
#4147=VECTOR('',#23862,1000.);
#4148=VECTOR('',#23863,1000.);
#4149=VECTOR('',#23864,1000.);
#4150=VECTOR('',#23865,1000.);
#4151=VECTOR('',#23866,1000.);
#4152=VECTOR('',#23867,1000.);
#4153=VECTOR('',#23870,1000.);
#4154=VECTOR('',#23871,1000.);
#4155=VECTOR('',#23872,1000.);
#4156=VECTOR('',#23873,1000.);
#4157=VECTOR('',#23874,1000.);
#4158=VECTOR('',#23875,1000.);
#4159=VECTOR('',#23878,1000.);
#4160=VECTOR('',#23879,1000.);
#4161=VECTOR('',#23882,1000.);
#4162=VECTOR('',#23883,1000.);
#4163=VECTOR('',#23886,1000.);
#4164=VECTOR('',#23889,1000.);
#4165=VECTOR('',#23890,1000.);
#4166=VECTOR('',#23891,1000.);
#4167=VECTOR('',#23892,1000.);
#4168=VECTOR('',#23893,1000.);
#4169=VECTOR('',#23894,1000.);
#4170=VECTOR('',#23897,1000.);
#4171=VECTOR('',#23898,1000.);
#4172=VECTOR('',#23899,1000.);
#4173=VECTOR('',#23900,1000.);
#4174=VECTOR('',#23901,1000.);
#4175=VECTOR('',#23902,1000.);
#4176=VECTOR('',#23905,1000.);
#4177=VECTOR('',#23906,1000.);
#4178=VECTOR('',#23907,1000.);
#4179=VECTOR('',#23910,1000.);
#4180=VECTOR('',#23911,1000.);
#4181=VECTOR('',#23914,1000.);
#4182=VECTOR('',#23915,1000.);
#4183=VECTOR('',#23918,1000.);
#4184=VECTOR('',#23919,1000.);
#4185=VECTOR('',#23922,1000.);
#4186=VECTOR('',#23923,1000.);
#4187=VECTOR('',#23926,1000.);
#4188=VECTOR('',#23929,1000.);
#4189=VECTOR('',#23932,1000.);
#4190=VECTOR('',#23935,1000.);
#4191=VECTOR('',#23942,1000.);
#4192=VECTOR('',#23943,1000.);
#4193=VECTOR('',#23946,1000.);
#4194=VECTOR('',#23949,1000.);
#4195=VECTOR('',#23950,1000.);
#4196=VECTOR('',#23951,1000.);
#4197=VECTOR('',#23954,1000.);
#4198=VECTOR('',#23955,1000.);
#4199=VECTOR('',#23958,1000.);
#4200=VECTOR('',#23959,1000.);
#4201=VECTOR('',#23962,1000.);
#4202=VECTOR('',#23963,1000.);
#4203=VECTOR('',#23966,1000.);
#4204=VECTOR('',#23967,1000.);
#4205=VECTOR('',#23970,1000.);
#4206=VECTOR('',#23973,1000.);
#4207=VECTOR('',#23976,1000.);
#4208=VECTOR('',#23981,1000.);
#4209=VECTOR('',#23984,1000.);
#4210=VECTOR('',#23985,1000.);
#4211=VECTOR('',#23988,1000.);
#4212=VECTOR('',#23989,1000.);
#4213=VECTOR('',#23990,1000.);
#4214=VECTOR('',#23993,1000.);
#4215=VECTOR('',#23994,1000.);
#4216=VECTOR('',#23997,1000.);
#4217=VECTOR('',#23998,1000.);
#4218=VECTOR('',#24001,1000.);
#4219=VECTOR('',#24002,1000.);
#4220=VECTOR('',#24005,1000.);
#4221=VECTOR('',#24006,1000.);
#4222=VECTOR('',#24009,1000.);
#4223=VECTOR('',#24012,1000.);
#4224=VECTOR('',#24021,1000.);
#4225=VECTOR('',#24024,1000.);
#4226=VECTOR('',#24033,1000.);
#4227=VECTOR('',#24034,1000.);
#4228=VECTOR('',#24037,1000.);
#4229=VECTOR('',#24048,1000.);
#4230=VECTOR('',#24051,1000.);
#4231=VECTOR('',#24052,1000.);
#4232=VECTOR('',#24053,1000.);
#4233=VECTOR('',#24056,1000.);
#4234=VECTOR('',#24061,1000.);
#4235=VECTOR('',#24062,1000.);
#4236=VECTOR('',#24063,1000.);
#4237=VECTOR('',#24066,1000.);
#4238=VECTOR('',#24067,1000.);
#4239=VECTOR('',#24072,1000.);
#4240=VECTOR('',#24075,1000.);
#4241=VECTOR('',#24078,1000.);
#4242=VECTOR('',#24085,1000.);
#4243=VECTOR('',#24086,1000.);
#4244=VECTOR('',#24089,1000.);
#4245=VECTOR('',#24092,1000.);
#4246=VECTOR('',#24093,1000.);
#4247=VECTOR('',#24096,1000.);
#4248=VECTOR('',#24097,1000.);
#4249=VECTOR('',#24098,1000.);
#4250=VECTOR('',#24101,1000.);
#4251=VECTOR('',#24102,1000.);
#4252=VECTOR('',#24105,1000.);
#4253=VECTOR('',#24106,1000.);
#4254=VECTOR('',#24109,1000.);
#4255=VECTOR('',#24110,1000.);
#4256=VECTOR('',#24113,1000.);
#4257=VECTOR('',#24114,1000.);
#4258=VECTOR('',#24117,1000.);
#4259=VECTOR('',#24120,1000.);
#4260=VECTOR('',#24123,1000.);
#4261=VECTOR('',#24126,1000.);
#4262=VECTOR('',#24131,1000.);
#4263=VECTOR('',#24132,1000.);
#4264=VECTOR('',#24137,1000.);
#4265=VECTOR('',#24138,1000.);
#4266=VECTOR('',#24139,1000.);
#4267=VECTOR('',#24142,1000.);
#4268=VECTOR('',#24143,1000.);
#4269=VECTOR('',#24146,1000.);
#4270=VECTOR('',#24147,1000.);
#4271=VECTOR('',#24150,1000.);
#4272=VECTOR('',#24151,1000.);
#4273=VECTOR('',#24154,1000.);
#4274=VECTOR('',#24155,1000.);
#4275=VECTOR('',#24158,1000.);
#4276=VECTOR('',#24161,1000.);
#4277=VECTOR('',#24162,1000.);
#4278=VECTOR('',#24163,1000.);
#4279=VECTOR('',#24166,1000.);
#4280=VECTOR('',#24167,1000.);
#4281=VECTOR('',#24170,1000.);
#4282=VECTOR('',#24171,1000.);
#4283=VECTOR('',#24174,1000.);
#4284=VECTOR('',#24175,1000.);
#4285=VECTOR('',#24178,1000.);
#4286=VECTOR('',#24179,1000.);
#4287=VECTOR('',#24182,1000.);
#4288=VECTOR('',#24187,1000.);
#4289=VECTOR('',#24188,1000.);
#4290=VECTOR('',#24189,1000.);
#4291=VECTOR('',#24190,1000.);
#4292=VECTOR('',#24191,1000.);
#4293=VECTOR('',#24192,1000.);
#4294=VECTOR('',#24197,1000.);
#4295=VECTOR('',#24198,1000.);
#4296=VECTOR('',#24199,1000.);
#4297=VECTOR('',#24200,1000.);
#4298=VECTOR('',#24201,1000.);
#4299=VECTOR('',#24202,1000.);
#4300=VECTOR('',#24205,1000.);
#4301=VECTOR('',#24206,1000.);
#4302=VECTOR('',#24207,1000.);
#4303=VECTOR('',#24210,1000.);
#4304=VECTOR('',#24211,1000.);
#4305=VECTOR('',#24212,1000.);
#4306=VECTOR('',#24213,1000.);
#4307=VECTOR('',#24214,1000.);
#4308=VECTOR('',#24217,1000.);
#4309=VECTOR('',#24218,1000.);
#4310=VECTOR('',#24219,1000.);
#4311=VECTOR('',#24222,1000.);
#4312=VECTOR('',#24223,1000.);
#4313=VECTOR('',#24224,1000.);
#4314=VECTOR('',#24227,1000.);
#4315=VECTOR('',#24228,1000.);
#4316=VECTOR('',#24231,1000.);
#4317=VECTOR('',#24232,1000.);
#4318=VECTOR('',#24235,1000.);
#4319=VECTOR('',#24236,1000.);
#4320=VECTOR('',#24239,1000.);
#4321=VECTOR('',#24240,1000.);
#4322=VECTOR('',#24243,1000.);
#4323=VECTOR('',#24248,1000.);
#4324=VECTOR('',#24249,1000.);
#4325=VECTOR('',#24250,1000.);
#4326=VECTOR('',#24251,1000.);
#4327=VECTOR('',#24254,1000.);
#4328=VECTOR('',#24255,1000.);
#4329=VECTOR('',#24258,1000.);
#4330=VECTOR('',#24259,1000.);
#4331=VECTOR('',#24262,1000.);
#4332=VECTOR('',#24263,1000.);
#4333=VECTOR('',#24266,1000.);
#4334=VECTOR('',#24269,1000.);
#4335=VECTOR('',#24270,1000.);
#4336=VECTOR('',#24273,1000.);
#4337=VECTOR('',#24278,1000.);
#4338=VECTOR('',#24283,1000.);
#4339=VECTOR('',#24288,1000.);
#4340=VECTOR('',#24289,1000.);
#4341=VECTOR('',#24294,1000.);
#4342=VECTOR('',#24297,1000.);
#4343=VECTOR('',#24300,1000.);
#4344=VECTOR('',#24301,1000.);
#4345=VECTOR('',#24302,1000.);
#4346=VECTOR('',#24307,1000.);
#4347=VECTOR('',#24308,1000.);
#4348=VECTOR('',#24311,1000.);
#4349=VECTOR('',#24312,1000.);
#4350=VECTOR('',#24315,1000.);
#4351=VECTOR('',#24318,1000.);
#4352=VECTOR('',#24325,1000.);
#4353=VECTOR('',#24330,1000.);
#4354=VECTOR('',#24335,1000.);
#4355=VECTOR('',#24336,1000.);
#4356=VECTOR('',#24337,1000.);
#4357=VECTOR('',#24340,1000.);
#4358=VECTOR('',#24341,1000.);
#4359=VECTOR('',#24344,1000.);
#4360=VECTOR('',#24345,1000.);
#4361=VECTOR('',#24348,1000.);
#4362=VECTOR('',#24349,1000.);
#4363=VECTOR('',#24352,1000.);
#4364=VECTOR('',#24353,1000.);
#4365=VECTOR('',#24356,1000.);
#4366=VECTOR('',#24359,1000.);
#4367=VECTOR('',#24362,1000.);
#4368=VECTOR('',#24365,1000.);
#4369=VECTOR('',#24366,1000.);
#4370=VECTOR('',#24367,1000.);
#4371=VECTOR('',#24370,1000.);
#4372=VECTOR('',#24371,1000.);
#4373=VECTOR('',#24374,1000.);
#4374=VECTOR('',#24375,1000.);
#4375=VECTOR('',#24378,1000.);
#4376=VECTOR('',#24381,1000.);
#4377=VECTOR('',#24386,1000.);
#4378=VECTOR('',#24389,1000.);
#4379=VECTOR('',#24390,1000.);
#4380=VECTOR('',#24393,1000.);
#4381=VECTOR('',#24398,1000.);
#4382=VECTOR('',#24403,1000.);
#4383=VECTOR('',#24406,1000.);
#4384=VECTOR('',#24407,1000.);
#4385=VECTOR('',#24412,1000.);
#4386=VECTOR('',#24417,1000.);
#4387=VECTOR('',#24418,1000.);
#4388=VECTOR('',#24423,1000.);
#4389=VECTOR('',#24428,1000.);
#4390=VECTOR('',#24429,1000.);
#4391=VECTOR('',#24432,1000.);
#4392=VECTOR('',#24435,1000.);
#4393=VECTOR('',#24440,1000.);
#4394=VECTOR('',#24477,1000.);
#4395=VECTOR('',#24478,1000.);
#4396=VECTOR('',#24479,1000.);
#4397=VECTOR('',#24480,1000.);
#4398=VECTOR('',#24481,1000.);
#4399=VECTOR('',#24482,1000.);
#4400=VECTOR('',#24485,1000.);
#4401=VECTOR('',#24486,1000.);
#4402=VECTOR('',#24489,1000.);
#4403=VECTOR('',#24490,1000.);
#4404=VECTOR('',#24491,1000.);
#4405=VECTOR('',#24494,1000.);
#4406=VECTOR('',#24495,1000.);
#4407=VECTOR('',#24498,1000.);
#4408=VECTOR('',#24499,1000.);
#4409=VECTOR('',#24500,1000.);
#4410=VECTOR('',#24503,1000.);
#4411=VECTOR('',#24504,1000.);
#4412=VECTOR('',#24507,1000.);
#4413=VECTOR('',#24508,1000.);
#4414=VECTOR('',#24509,1000.);
#4415=VECTOR('',#24510,1000.);
#4416=VECTOR('',#24511,1000.);
#4417=VECTOR('',#24512,1000.);
#4418=VECTOR('',#24513,1000.);
#4419=VECTOR('',#24514,1000.);
#4420=VECTOR('',#24515,1000.);
#4421=VECTOR('',#24516,1000.);
#4422=VECTOR('',#24519,1000.);
#4423=VECTOR('',#24520,1000.);
#4424=VECTOR('',#24523,1000.);
#4425=VECTOR('',#24524,1000.);
#4426=VECTOR('',#24525,1000.);
#4427=VECTOR('',#24528,1000.);
#4428=VECTOR('',#24529,1000.);
#4429=VECTOR('',#24532,1000.);
#4430=VECTOR('',#24533,1000.);
#4431=VECTOR('',#24534,1000.);
#4432=VECTOR('',#24537,1000.);
#4433=VECTOR('',#24538,1000.);
#4434=VECTOR('',#24541,1000.);
#4435=VECTOR('',#24542,1000.);
#4436=VECTOR('',#24543,1000.);
#4437=VECTOR('',#24544,1000.);
#4438=VECTOR('',#24545,1000.);
#4439=VECTOR('',#24548,1000.);
#4440=VECTOR('',#24549,1000.);
#4441=VECTOR('',#24550,1000.);
#4442=VECTOR('',#24555,1000.);
#4443=VECTOR('',#24556,1000.);
#4444=VECTOR('',#24561,1000.);
#4445=VECTOR('',#24562,1000.);
#4446=VECTOR('',#24567,1000.);
#4447=VECTOR('',#24568,1000.);
#4448=VECTOR('',#24571,1000.);
#4449=VECTOR('',#24572,1000.);
#4450=VECTOR('',#24573,1000.);
#4451=VECTOR('',#24574,1000.);
#4452=VECTOR('',#24575,1000.);
#4453=VECTOR('',#24576,1000.);
#4454=VECTOR('',#24579,1000.);
#4455=VECTOR('',#24580,1000.);
#4456=VECTOR('',#24583,1000.);
#4457=VECTOR('',#24586,1000.);
#4458=VECTOR('',#24589,1000.);
#4459=VECTOR('',#24590,1000.);
#4460=VECTOR('',#24593,1000.);
#4461=VECTOR('',#24594,1000.);
#4462=VECTOR('',#24597,1000.);
#4463=VECTOR('',#24598,1000.);
#4464=VECTOR('',#24599,1000.);
#4465=VECTOR('',#24600,1000.);
#4466=VECTOR('',#24601,1000.);
#4467=VECTOR('',#24624,1000.);
#4468=VECTOR('',#24625,1000.);
#4469=VECTOR('',#24626,1000.);
#4470=VECTOR('',#24627,1000.);
#4471=VECTOR('',#24630,1000.);
#4472=VECTOR('',#24631,1000.);
#4473=VECTOR('',#24632,1000.);
#4474=VECTOR('',#24635,1000.);
#4475=VECTOR('',#24636,1000.);
#4476=VECTOR('',#24639,1000.);
#4477=VECTOR('',#24642,1000.);
#4478=VECTOR('',#24645,1000.);
#4479=VECTOR('',#24646,1000.);
#4480=VECTOR('',#24649,1000.);
#4481=VECTOR('',#24650,1000.);
#4482=VECTOR('',#24651,1000.);
#4483=VECTOR('',#24654,1000.);
#4484=VECTOR('',#24655,1000.);
#4485=VECTOR('',#24658,1000.);
#4486=VECTOR('',#24659,1000.);
#4487=VECTOR('',#24662,1000.);
#4488=VECTOR('',#24663,1000.);
#4489=VECTOR('',#24664,1000.);
#4490=VECTOR('',#24667,1000.);
#4491=VECTOR('',#24668,1000.);
#4492=VECTOR('',#24669,1000.);
#4493=VECTOR('',#24672,1000.);
#4494=VECTOR('',#24673,1000.);
#4495=VECTOR('',#24676,1000.);
#4496=VECTOR('',#24677,1000.);
#4497=VECTOR('',#24680,1000.);
#4498=VECTOR('',#24683,1000.);
#4499=VECTOR('',#24686,1000.);
#4500=VECTOR('',#24689,1000.);
#4501=VECTOR('',#24690,1000.);
#4502=VECTOR('',#24691,1000.);
#4503=VECTOR('',#24692,1000.);
#4504=VECTOR('',#24695,1000.);
#4505=VECTOR('',#24696,1000.);
#4506=VECTOR('',#24699,1000.);
#4507=VECTOR('',#24700,1000.);
#4508=VECTOR('',#24701,1000.);
#4509=VECTOR('',#24704,1000.);
#4510=VECTOR('',#24705,1000.);
#4511=VECTOR('',#24706,1000.);
#4512=VECTOR('',#24709,1000.);
#4513=VECTOR('',#24710,1000.);
#4514=VECTOR('',#24713,1000.);
#4515=VECTOR('',#24714,1000.);
#4516=VECTOR('',#24717,1000.);
#4517=VECTOR('',#24718,1000.);
#4518=VECTOR('',#24721,1000.);
#4519=VECTOR('',#24722,1000.);
#4520=VECTOR('',#24725,1000.);
#4521=VECTOR('',#24726,1000.);
#4522=VECTOR('',#24729,1000.);
#4523=VECTOR('',#24730,1000.);
#4524=VECTOR('',#24733,1000.);
#4525=VECTOR('',#24734,1000.);
#4526=VECTOR('',#24737,1000.);
#4527=VECTOR('',#24738,1000.);
#4528=VECTOR('',#24741,1000.);
#4529=VECTOR('',#24742,1000.);
#4530=VECTOR('',#24745,1000.);
#4531=VECTOR('',#24746,1000.);
#4532=VECTOR('',#24749,1000.);
#4533=VECTOR('',#24772,3.5);
#4534=VECTOR('',#24785,1.61);
#4535=VECTOR('',#24790,2.);
#4536=VECTOR('',#24797,1000.);
#4537=VECTOR('',#24798,1000.);
#4538=VECTOR('',#24801,1000.);
#4539=VECTOR('',#24802,1000.);
#4540=VECTOR('',#24805,1000.);
#4541=VECTOR('',#24806,1000.);
#4542=VECTOR('',#24809,1000.);
#4543=VECTOR('',#24810,1000.);
#4544=VECTOR('',#24813,1000.);
#4545=VECTOR('',#24814,1000.);
#4546=VECTOR('',#24817,1000.);
#4547=VECTOR('',#24818,1000.);
#4548=VECTOR('',#24847,1000.);
#4549=VECTOR('',#24848,1000.);
#4550=VECTOR('',#24851,1000.);
#4551=VECTOR('',#24854,1000.);
#4552=VECTOR('',#24857,1000.);
#4553=VECTOR('',#24860,1000.);
#4554=CYLINDRICAL_SURFACE('',#18360,35.);
#4555=CYLINDRICAL_SURFACE('',#18381,2.5);
#4556=CYLINDRICAL_SURFACE('',#18384,2.49999999999997);
#4557=CYLINDRICAL_SURFACE('',#18387,2.5);
#4558=CYLINDRICAL_SURFACE('',#18390,2.5);
#4559=CYLINDRICAL_SURFACE('',#18393,2.49999999999997);
#4560=CYLINDRICAL_SURFACE('',#18396,2.5);
#4561=CYLINDRICAL_SURFACE('',#18399,2.5);
#4562=CYLINDRICAL_SURFACE('',#18402,2.5);
#4563=CYLINDRICAL_SURFACE('',#18405,19.);
#4564=CYLINDRICAL_SURFACE('',#18407,19.);
#4565=CYLINDRICAL_SURFACE('',#18409,15.);
#4566=CYLINDRICAL_SURFACE('',#18411,15.);
#4567=CYLINDRICAL_SURFACE('',#18413,25.);
#4568=CYLINDRICAL_SURFACE('',#18415,2.5);
#4569=CYLINDRICAL_SURFACE('',#18418,2.5);
#4570=CYLINDRICAL_SURFACE('',#18421,2.5);
#4571=CYLINDRICAL_SURFACE('',#18424,2.5);
#4572=CYLINDRICAL_SURFACE('',#18427,2.5);
#4573=CYLINDRICAL_SURFACE('',#18430,2.5);
#4574=CYLINDRICAL_SURFACE('',#18433,2.5);
#4575=CYLINDRICAL_SURFACE('',#18436,2.5);
#4576=CYLINDRICAL_SURFACE('',#18439,2.50000000000001);
#4577=CYLINDRICAL_SURFACE('',#18442,2.5);
#4578=CYLINDRICAL_SURFACE('',#18445,2.5);
#4579=CYLINDRICAL_SURFACE('',#18448,2.5);
#4580=CYLINDRICAL_SURFACE('',#18451,2.5);
#4581=CYLINDRICAL_SURFACE('',#18454,2.5);
#4582=CYLINDRICAL_SURFACE('',#18457,2.5);
#4583=CYLINDRICAL_SURFACE('',#18460,250.);
#4584=CYLINDRICAL_SURFACE('',#18462,275.);
#4585=CYLINDRICAL_SURFACE('',#18465,240.);
#4586=CYLINDRICAL_SURFACE('',#18482,5.);
#4587=CYLINDRICAL_SURFACE('',#18484,5.);
#4588=CYLINDRICAL_SURFACE('',#18486,5.00000000000003);
#4589=CYLINDRICAL_SURFACE('',#18488,5.);
#4590=CYLINDRICAL_SURFACE('',#18500,5.);
#4591=CYLINDRICAL_SURFACE('',#18502,5.);
#4592=CYLINDRICAL_SURFACE('',#18504,5.);
#4593=CYLINDRICAL_SURFACE('',#18506,5.00000000000003);
#4594=CYLINDRICAL_SURFACE('',#18537,206.);
#4595=CYLINDRICAL_SURFACE('',#18540,145.404667636179);
#4596=CYLINDRICAL_SURFACE('',#18543,5.);
#4597=CYLINDRICAL_SURFACE('',#18545,147.404667636179);
#4598=CYLINDRICAL_SURFACE('',#18555,145.404667636179);
#4599=CYLINDRICAL_SURFACE('',#18557,206.);
#4600=CYLINDRICAL_SURFACE('',#18561,204.);
#4601=CYLINDRICAL_SURFACE('',#18562,204.);
#4602=CYLINDRICAL_SURFACE('',#18563,204.);
#4603=CYLINDRICAL_SURFACE('',#18564,204.);
#4604=CYLINDRICAL_SURFACE('',#18565,204.);
#4605=CYLINDRICAL_SURFACE('',#18566,204.);
#4606=CYLINDRICAL_SURFACE('',#18567,204.);
#4607=CYLINDRICAL_SURFACE('',#18568,204.);
#4608=CYLINDRICAL_SURFACE('',#18569,206.);
#4609=CYLINDRICAL_SURFACE('',#18572,145.404667636179);
#4610=CYLINDRICAL_SURFACE('',#18575,5.);
#4611=CYLINDRICAL_SURFACE('',#18577,147.404667636179);
#4612=CYLINDRICAL_SURFACE('',#18589,145.404667636179);
#4613=CYLINDRICAL_SURFACE('',#18591,206.);
#4614=CYLINDRICAL_SURFACE('',#18595,204.);
#4615=CYLINDRICAL_SURFACE('',#18596,204.);
#4616=CYLINDRICAL_SURFACE('',#18597,204.);
#4617=CYLINDRICAL_SURFACE('',#18598,204.);
#4618=CYLINDRICAL_SURFACE('',#18599,204.);
#4619=CYLINDRICAL_SURFACE('',#18600,204.);
#4620=CYLINDRICAL_SURFACE('',#18601,204.);
#4621=CYLINDRICAL_SURFACE('',#18602,204.);
#4622=CYLINDRICAL_SURFACE('',#18603,10.);
#4623=CYLINDRICAL_SURFACE('',#18606,10.);
#4624=CYLINDRICAL_SURFACE('',#18609,27.9488084273619);
#4625=CYLINDRICAL_SURFACE('',#18612,17.4625);
#4626=CYLINDRICAL_SURFACE('',#18615,25.);
#4627=CYLINDRICAL_SURFACE('',#18618,204.);
#4628=CYLINDRICAL_SURFACE('',#18621,200.);
#4629=CYLINDRICAL_SURFACE('',#18650,25.);
#4630=CYLINDRICAL_SURFACE('',#18652,25.);
#4631=CYLINDRICAL_SURFACE('',#18654,25.);
#4632=CYLINDRICAL_SURFACE('',#18656,25.);
#4633=CYLINDRICAL_SURFACE('',#18658,25.);
#4634=CYLINDRICAL_SURFACE('',#18660,25.);
#4635=CYLINDRICAL_SURFACE('',#18662,25.);
#4636=CYLINDRICAL_SURFACE('',#18664,25.);
#4637=CYLINDRICAL_SURFACE('',#18668,122.05461305459);
#4638=CYLINDRICAL_SURFACE('',#18670,77.4625);
#4639=CYLINDRICAL_SURFACE('',#18672,122.05461305459);
#4640=CYLINDRICAL_SURFACE('',#18674,122.05461305459);
#4641=CYLINDRICAL_SURFACE('',#18676,77.4625);
#4642=CYLINDRICAL_SURFACE('',#18678,122.05461305459);
#4643=CYLINDRICAL_SURFACE('',#18685,27.9488084273619);
#4644=CYLINDRICAL_SURFACE('',#18716,10.);
#4645=CYLINDRICAL_SURFACE('',#18717,10.);
#4646=CYLINDRICAL_SURFACE('',#18738,14.);
#4647=CYLINDRICAL_SURFACE('',#18740,14.);
#4648=CYLINDRICAL_SURFACE('',#18744,15.);
#4649=CYLINDRICAL_SURFACE('',#18746,15.);
#4650=CYLINDRICAL_SURFACE('',#18750,147.404667636179);
#4651=CYLINDRICAL_SURFACE('',#18751,148.404667636179);
#4652=CYLINDRICAL_SURFACE('',#18753,6.75000000000001);
#4653=CYLINDRICAL_SURFACE('',#18756,6.74999999999998);
#4654=CYLINDRICAL_SURFACE('',#18759,6.74999999999998);
#4655=CYLINDRICAL_SURFACE('',#18762,6.75000000000001);
#4656=CYLINDRICAL_SURFACE('',#18794,96.161193339026);
#4657=CYLINDRICAL_SURFACE('',#18797,2.5);
#4658=CYLINDRICAL_SURFACE('',#18800,2.5);
#4659=CYLINDRICAL_SURFACE('',#18803,2.5);
#4660=CYLINDRICAL_SURFACE('',#18806,2.5);
#4661=CYLINDRICAL_SURFACE('',#18809,2.5);
#4662=CYLINDRICAL_SURFACE('',#18812,2.5);
#4663=CYLINDRICAL_SURFACE('',#18815,2.5);
#4664=CYLINDRICAL_SURFACE('',#18818,2.5);
#4665=CYLINDRICAL_SURFACE('',#18821,2.50000000000001);
#4666=CYLINDRICAL_SURFACE('',#18824,2.5);
#4667=CYLINDRICAL_SURFACE('',#18827,2.5);
#4668=CYLINDRICAL_SURFACE('',#18830,2.5);
#4669=CYLINDRICAL_SURFACE('',#18833,2.5);
#4670=CYLINDRICAL_SURFACE('',#18836,2.5);
#4671=CYLINDRICAL_SURFACE('',#18839,2.5);
#4672=CYLINDRICAL_SURFACE('',#18842,275.);
#4673=CYLINDRICAL_SURFACE('',#18847,96.161193339026);
#4674=CYLINDRICAL_SURFACE('',#18876,55.);
#4675=CYLINDRICAL_SURFACE('',#18910,6.75000000000001);
#4676=CYLINDRICAL_SURFACE('',#18913,6.75);
#4677=CYLINDRICAL_SURFACE('',#18916,6.75000000000001);
#4678=CYLINDRICAL_SURFACE('',#18919,6.75);
#4679=CYLINDRICAL_SURFACE('',#18922,7.00000000000001);
#4680=CYLINDRICAL_SURFACE('',#18927,27.5);
#4681=CYLINDRICAL_SURFACE('',#18935,22.);
#4682=CYLINDRICAL_SURFACE('',#18938,7.);
#4683=CYLINDRICAL_SURFACE('',#18941,7.);
#4684=CYLINDRICAL_SURFACE('',#18946,7.);
#4685=CYLINDRICAL_SURFACE('',#18953,80.);
#4686=CYLINDRICAL_SURFACE('',#18956,40.);
#4687=CYLINDRICAL_SURFACE('',#18959,12.);
#4688=CYLINDRICAL_SURFACE('',#18960,12.);
#4689=CYLINDRICAL_SURFACE('',#18961,12.);
#4690=CYLINDRICAL_SURFACE('',#18964,12.);
#4691=CYLINDRICAL_SURFACE('',#18966,12.);
#4692=CYLINDRICAL_SURFACE('',#18967,53.);
#4693=CYLINDRICAL_SURFACE('',#18971,4.5);
#4694=CYLINDRICAL_SURFACE('',#18974,4.5);
#4695=CYLINDRICAL_SURFACE('',#18977,4.5);
#4696=CYLINDRICAL_SURFACE('',#18980,4.5);
#4697=CYLINDRICAL_SURFACE('',#18983,20.);
#4698=CYLINDRICAL_SURFACE('',#18986,12.);
#4699=CYLINDRICAL_SURFACE('',#18988,10.);
#4700=CYLINDRICAL_SURFACE('',#18990,12.);
#4701=CYLINDRICAL_SURFACE('',#19003,7.00000000000001);
#4702=CYLINDRICAL_SURFACE('',#19009,12.);
#4703=CYLINDRICAL_SURFACE('',#19012,68.);
#4704=CYLINDRICAL_SURFACE('',#19018,4.);
#4705=CYLINDRICAL_SURFACE('',#19021,4.);
#4706=CYLINDRICAL_SURFACE('',#19024,4.);
#4707=CYLINDRICAL_SURFACE('',#19027,4.);
#4708=CYLINDRICAL_SURFACE('',#19030,17.4625);
#4709=CYLINDRICAL_SURFACE('',#19037,7.99999999999999);
#4710=CYLINDRICAL_SURFACE('',#19040,8.00000000000001);
#4711=CYLINDRICAL_SURFACE('',#19045,7.00000000000001);
#4712=CYLINDRICAL_SURFACE('',#19048,7.00000000000001);
#4713=CYLINDRICAL_SURFACE('',#19051,3.);
#4714=CYLINDRICAL_SURFACE('',#19054,3.00000000000307);
#4715=CYLINDRICAL_SURFACE('',#19057,3.0000000000021);
#4716=CYLINDRICAL_SURFACE('',#19060,2.99999999999927);
#4717=CYLINDRICAL_SURFACE('',#19063,68.);
#4718=CYLINDRICAL_SURFACE('',#19066,6.7500000000354);
#4719=CYLINDRICAL_SURFACE('',#19075,5.5);
#4720=CYLINDRICAL_SURFACE('',#19084,8.80000000000425);
#4721=CYLINDRICAL_SURFACE('',#19087,8.80000000000425);
#4722=CYLINDRICAL_SURFACE('',#19092,5.5);
#4723=CYLINDRICAL_SURFACE('',#19096,179.5);
#4724=CYLINDRICAL_SURFACE('',#19132,7.00000000000001);
#4725=CYLINDRICAL_SURFACE('',#19145,7.00000000000001);
#4726=CYLINDRICAL_SURFACE('',#19158,7.00000000000001);
#4727=CYLINDRICAL_SURFACE('',#19173,7.00000000000001);
#4728=CYLINDRICAL_SURFACE('',#19177,16.);
#4729=CYLINDRICAL_SURFACE('',#19180,16.);
#4730=CYLINDRICAL_SURFACE('',#19182,179.5);
#4731=CYLINDRICAL_SURFACE('',#19184,16.);
#4732=CYLINDRICAL_SURFACE('',#19187,16.);
#4733=CYLINDRICAL_SURFACE('',#19189,179.5);
#4734=CYLINDRICAL_SURFACE('',#19191,16.);
#4735=CYLINDRICAL_SURFACE('',#19194,16.);
#4736=CYLINDRICAL_SURFACE('',#19196,16.);
#4737=CYLINDRICAL_SURFACE('',#19199,16.);
#4738=CYLINDRICAL_SURFACE('',#19201,179.5);
#4739=CYLINDRICAL_SURFACE('',#19227,7.00000000000001);
#4740=CYLINDRICAL_SURFACE('',#19228,7.00000000000001);
#4741=CYLINDRICAL_SURFACE('',#19231,7.00000000000001);
#4742=CYLINDRICAL_SURFACE('',#19236,7.00000000000001);
#4743=CYLINDRICAL_SURFACE('',#19240,80.5);
#4744=CYLINDRICAL_SURFACE('',#19244,80.5);
#4745=CYLINDRICAL_SURFACE('',#19248,80.5);
#4746=CYLINDRICAL_SURFACE('',#19252,80.5);
#4747=CYLINDRICAL_SURFACE('',#19266,7.00000000000001);
#4748=CYLINDRICAL_SURFACE('',#19269,7.00000000000001);
#4749=CYLINDRICAL_SURFACE('',#19272,7.00000000000001);
#4750=CYLINDRICAL_SURFACE('',#19275,7.00000000000001);
#4751=CYLINDRICAL_SURFACE('',#19347,4.);
#4752=CYLINDRICAL_SURFACE('',#19350,4.);
#4753=CYLINDRICAL_SURFACE('',#19352,4.);
#4754=CYLINDRICAL_SURFACE('',#19354,4.);
#4755=CYLINDRICAL_SURFACE('',#19385,1.);
#4756=CYLINDRICAL_SURFACE('',#19386,1.);
#4757=CYLINDRICAL_SURFACE('',#19387,1.);
#4758=CYLINDRICAL_SURFACE('',#19388,1.);
#4759=CYLINDRICAL_SURFACE('',#19435,68.);
#4760=CYLINDRICAL_SURFACE('',#19438,77.);
#4761=CYLINDRICAL_SURFACE('',#19444,68.);
#4762=CYLINDRICAL_SURFACE('',#19446,77.);
#4763=CYLINDRICAL_SURFACE('',#19449,68.);
#4764=CYLINDRICAL_SURFACE('',#19452,77.);
#4765=CYLINDRICAL_SURFACE('',#19457,77.);
#4766=CYLINDRICAL_SURFACE('',#19466,5.);
#4767=CYLINDRICAL_SURFACE('',#19479,5.);
#4768=CYLINDRICAL_SURFACE('',#19488,5.);
#4769=CYLINDRICAL_SURFACE('',#19493,5.);
#4770=CYLINDRICAL_SURFACE('',#19506,77.);
#4771=CYLINDRICAL_SURFACE('',#19509,4.);
#4772=CYLINDRICAL_SURFACE('',#19514,4.);
#4773=CYLINDRICAL_SURFACE('',#19519,77.);
#4774=CYLINDRICAL_SURFACE('',#19522,4.);
#4775=CYLINDRICAL_SURFACE('',#19527,4.);
#4776=CYLINDRICAL_SURFACE('',#19532,77.);
#4777=CYLINDRICAL_SURFACE('',#19535,4.);
#4778=CYLINDRICAL_SURFACE('',#19540,4.);
#4779=CYLINDRICAL_SURFACE('',#19545,77.);
#4780=CYLINDRICAL_SURFACE('',#19548,4.);
#4781=CYLINDRICAL_SURFACE('',#19553,4.);
#4782=CYLINDRICAL_SURFACE('',#19604,76.5);
#4783=CYLINDRICAL_SURFACE('',#19606,68.);
#4784=CYLINDRICAL_SURFACE('',#19608,76.5);
#4785=CYLINDRICAL_SURFACE('',#19611,76.5);
#4786=CYLINDRICAL_SURFACE('',#19613,68.);
#4787=CYLINDRICAL_SURFACE('',#19615,76.5);
#4788=CYLINDRICAL_SURFACE('',#19617,68.);
#4789=CYLINDRICAL_SURFACE('',#19627,12.);
#4790=CYLINDRICAL_SURFACE('',#19634,10.);
#4791=CYLINDRICAL_SURFACE('',#19644,4.5);
#4792=CYLINDRICAL_SURFACE('',#19682,2.);
#4793=CYLINDRICAL_SURFACE('',#19686,2.);
#4794=CYLINDRICAL_SURFACE('',#19706,10.);
#4795=CYLINDRICAL_SURFACE('',#19717,10.);
#4796=CYLINDRICAL_SURFACE('',#19728,12.);
#4797=CYLINDRICAL_SURFACE('',#19729,12.);
#4798=CYLINDRICAL_SURFACE('',#19730,12.);
#4799=CYLINDRICAL_SURFACE('',#19734,2.);
#4800=CYLINDRICAL_SURFACE('',#19738,2.);
#4801=CYLINDRICAL_SURFACE('',#19741,12.);
#4802=CYLINDRICAL_SURFACE('',#19742,12.);
#4803=CYLINDRICAL_SURFACE('',#19743,12.);
#4804=CYLINDRICAL_SURFACE('',#19752,10.);
#4805=CYLINDRICAL_SURFACE('',#19756,6.);
#4806=CYLINDRICAL_SURFACE('',#19766,10.);
#4807=CYLINDRICAL_SURFACE('',#19804,2.5);
#4808=CYLINDRICAL_SURFACE('',#19810,6.00000000000001);
#4809=CYLINDRICAL_SURFACE('',#19813,6.00000000000001);
#4810=CYLINDRICAL_SURFACE('',#19816,2.5);
#4811=CYLINDRICAL_SURFACE('',#19819,6.00000000000001);
#4812=CYLINDRICAL_SURFACE('',#19846,6.);
#4813=CYLINDRICAL_SURFACE('',#19850,6.);
#4814=CYLINDRICAL_SURFACE('',#19862,23.5);
#4815=CYLINDRICAL_SURFACE('',#19871,20.5);
#4816=CYLINDRICAL_SURFACE('',#19889,12.);
#4817=CYLINDRICAL_SURFACE('',#19891,12.);
#4818=CYLINDRICAL_SURFACE('',#19893,12.);
#4819=CYLINDRICAL_SURFACE('',#19902,12.);
#4820=CYLINDRICAL_SURFACE('',#19950,3.5);
#4821=CYLINDRICAL_SURFACE('',#19961,2.);
#4822=FACE_OUTER_BOUND('',#5815,.T.);
#4823=FACE_OUTER_BOUND('',#5816,.T.);
#4824=FACE_OUTER_BOUND('',#5817,.T.);
#4825=FACE_OUTER_BOUND('',#5818,.T.);
#4826=FACE_OUTER_BOUND('',#5819,.T.);
#4827=FACE_OUTER_BOUND('',#5820,.T.);
#4828=FACE_OUTER_BOUND('',#5821,.T.);
#4829=FACE_OUTER_BOUND('',#5822,.T.);
#4830=FACE_OUTER_BOUND('',#5823,.T.);
#4831=FACE_OUTER_BOUND('',#5824,.T.);
#4832=FACE_OUTER_BOUND('',#5825,.T.);
#4833=FACE_OUTER_BOUND('',#5826,.T.);
#4834=FACE_OUTER_BOUND('',#5827,.T.);
#4835=FACE_OUTER_BOUND('',#5828,.T.);
#4836=FACE_OUTER_BOUND('',#5829,.T.);
#4837=FACE_OUTER_BOUND('',#5830,.T.);
#4838=FACE_OUTER_BOUND('',#5831,.T.);
#4839=FACE_OUTER_BOUND('',#5832,.T.);
#4840=FACE_OUTER_BOUND('',#5833,.T.);
#4841=FACE_OUTER_BOUND('',#5834,.T.);
#4842=FACE_OUTER_BOUND('',#5835,.T.);
#4843=FACE_OUTER_BOUND('',#5836,.T.);
#4844=FACE_OUTER_BOUND('',#5837,.T.);
#4845=FACE_OUTER_BOUND('',#5838,.T.);
#4846=FACE_OUTER_BOUND('',#5839,.T.);
#4847=FACE_OUTER_BOUND('',#5840,.T.);
#4848=FACE_OUTER_BOUND('',#5841,.T.);
#4849=FACE_OUTER_BOUND('',#5842,.T.);
#4850=FACE_OUTER_BOUND('',#5843,.T.);
#4851=FACE_OUTER_BOUND('',#5844,.T.);
#4852=FACE_OUTER_BOUND('',#5845,.T.);
#4853=FACE_OUTER_BOUND('',#5846,.T.);
#4854=FACE_OUTER_BOUND('',#5849,.T.);
#4855=FACE_OUTER_BOUND('',#5850,.T.);
#4856=FACE_OUTER_BOUND('',#5853,.T.);
#4857=FACE_OUTER_BOUND('',#5855,.T.);
#4858=FACE_OUTER_BOUND('',#5872,.T.);
#4859=FACE_OUTER_BOUND('',#5889,.T.);
#4860=FACE_OUTER_BOUND('',#5891,.T.);
#4861=FACE_OUTER_BOUND('',#5897,.T.);
#4862=FACE_OUTER_BOUND('',#5903,.T.);
#4863=FACE_OUTER_BOUND('',#5904,.T.);
#4864=FACE_OUTER_BOUND('',#5905,.T.);
#4865=FACE_OUTER_BOUND('',#5906,.T.);
#4866=FACE_OUTER_BOUND('',#5907,.T.);
#4867=FACE_OUTER_BOUND('',#5908,.T.);
#4868=FACE_OUTER_BOUND('',#5909,.T.);
#4869=FACE_OUTER_BOUND('',#5910,.T.);
#4870=FACE_OUTER_BOUND('',#5911,.T.);
#4871=FACE_OUTER_BOUND('',#5917,.T.);
#4872=FACE_OUTER_BOUND('',#5923,.T.);
#4873=FACE_OUTER_BOUND('',#5924,.T.);
#4874=FACE_OUTER_BOUND('',#5925,.T.);
#4875=FACE_OUTER_BOUND('',#5926,.T.);
#4876=FACE_OUTER_BOUND('',#5927,.T.);
#4877=FACE_OUTER_BOUND('',#5928,.T.);
#4878=FACE_OUTER_BOUND('',#5929,.T.);
#4879=FACE_OUTER_BOUND('',#5930,.T.);
#4880=FACE_OUTER_BOUND('',#5931,.T.);
#4881=FACE_OUTER_BOUND('',#5933,.T.);
#4882=FACE_OUTER_BOUND('',#5934,.T.);
#4883=FACE_OUTER_BOUND('',#5935,.T.);
#4884=FACE_OUTER_BOUND('',#5936,.T.);
#4885=FACE_OUTER_BOUND('',#5937,.T.);
#4886=FACE_OUTER_BOUND('',#5938,.T.);
#4887=FACE_OUTER_BOUND('',#5939,.T.);
#4888=FACE_OUTER_BOUND('',#5940,.T.);
#4889=FACE_OUTER_BOUND('',#5941,.T.);
#4890=FACE_OUTER_BOUND('',#5942,.T.);
#4891=FACE_OUTER_BOUND('',#5943,.T.);
#4892=FACE_OUTER_BOUND('',#5944,.T.);
#4893=FACE_OUTER_BOUND('',#5945,.T.);
#4894=FACE_OUTER_BOUND('',#5946,.T.);
#4895=FACE_OUTER_BOUND('',#5947,.T.);
#4896=FACE_OUTER_BOUND('',#5948,.T.);
#4897=FACE_OUTER_BOUND('',#5949,.T.);
#4898=FACE_OUTER_BOUND('',#5950,.T.);
#4899=FACE_OUTER_BOUND('',#5951,.T.);
#4900=FACE_OUTER_BOUND('',#5952,.T.);
#4901=FACE_OUTER_BOUND('',#5953,.T.);
#4902=FACE_OUTER_BOUND('',#5954,.T.);
#4903=FACE_OUTER_BOUND('',#5955,.T.);
#4904=FACE_OUTER_BOUND('',#5956,.T.);
#4905=FACE_OUTER_BOUND('',#5957,.T.);
#4906=FACE_OUTER_BOUND('',#5958,.T.);
#4907=FACE_OUTER_BOUND('',#5959,.T.);
#4908=FACE_OUTER_BOUND('',#5960,.T.);
#4909=FACE_OUTER_BOUND('',#5961,.T.);
#4910=FACE_OUTER_BOUND('',#5962,.T.);
#4911=FACE_OUTER_BOUND('',#5963,.T.);
#4912=FACE_OUTER_BOUND('',#5964,.T.);
#4913=FACE_OUTER_BOUND('',#5966,.T.);
#4914=FACE_OUTER_BOUND('',#5968,.T.);
#4915=FACE_OUTER_BOUND('',#5969,.T.);
#4916=FACE_OUTER_BOUND('',#5970,.T.);
#4917=FACE_OUTER_BOUND('',#5971,.T.);
#4918=FACE_OUTER_BOUND('',#5972,.T.);
#4919=FACE_OUTER_BOUND('',#5973,.T.);
#4920=FACE_OUTER_BOUND('',#5974,.T.);
#4921=FACE_OUTER_BOUND('',#5975,.T.);
#4922=FACE_OUTER_BOUND('',#5976,.T.);
#4923=FACE_OUTER_BOUND('',#5977,.T.);
#4924=FACE_OUTER_BOUND('',#5978,.T.);
#4925=FACE_OUTER_BOUND('',#5979,.T.);
#4926=FACE_OUTER_BOUND('',#5980,.T.);
#4927=FACE_OUTER_BOUND('',#5981,.T.);
#4928=FACE_OUTER_BOUND('',#5982,.T.);
#4929=FACE_OUTER_BOUND('',#5983,.T.);
#4930=FACE_OUTER_BOUND('',#5984,.T.);
#4931=FACE_OUTER_BOUND('',#5985,.T.);
#4932=FACE_OUTER_BOUND('',#5987,.T.);
#4933=FACE_OUTER_BOUND('',#5989,.T.);
#4934=FACE_OUTER_BOUND('',#5990,.T.);
#4935=FACE_OUTER_BOUND('',#5991,.T.);
#4936=FACE_OUTER_BOUND('',#5992,.T.);
#4937=FACE_OUTER_BOUND('',#5993,.T.);
#4938=FACE_OUTER_BOUND('',#5996,.T.);
#4939=FACE_OUTER_BOUND('',#5999,.T.);
#4940=FACE_OUTER_BOUND('',#6000,.T.);
#4941=FACE_OUTER_BOUND('',#6001,.T.);
#4942=FACE_OUTER_BOUND('',#6002,.T.);
#4943=FACE_OUTER_BOUND('',#6003,.T.);
#4944=FACE_OUTER_BOUND('',#6004,.T.);
#4945=FACE_OUTER_BOUND('',#6005,.T.);
#4946=FACE_OUTER_BOUND('',#6006,.T.);
#4947=FACE_OUTER_BOUND('',#6007,.T.);
#4948=FACE_OUTER_BOUND('',#6008,.T.);
#4949=FACE_OUTER_BOUND('',#6009,.T.);
#4950=FACE_OUTER_BOUND('',#6011,.T.);
#4951=FACE_OUTER_BOUND('',#6017,.T.);
#4952=FACE_OUTER_BOUND('',#6019,.T.);
#4953=FACE_OUTER_BOUND('',#6020,.T.);
#4954=FACE_OUTER_BOUND('',#6021,.T.);
#4955=FACE_OUTER_BOUND('',#6022,.T.);
#4956=FACE_OUTER_BOUND('',#6023,.T.);
#4957=FACE_OUTER_BOUND('',#6024,.T.);
#4958=FACE_OUTER_BOUND('',#6025,.T.);
#4959=FACE_OUTER_BOUND('',#6026,.T.);
#4960=FACE_OUTER_BOUND('',#6027,.T.);
#4961=FACE_OUTER_BOUND('',#6029,.T.);
#4962=FACE_OUTER_BOUND('',#6031,.T.);
#4963=FACE_OUTER_BOUND('',#6032,.T.);
#4964=FACE_OUTER_BOUND('',#6033,.T.);
#4965=FACE_OUTER_BOUND('',#6034,.T.);
#4966=FACE_OUTER_BOUND('',#6035,.T.);
#4967=FACE_OUTER_BOUND('',#6036,.T.);
#4968=FACE_OUTER_BOUND('',#6037,.T.);
#4969=FACE_OUTER_BOUND('',#6039,.T.);
#4970=FACE_OUTER_BOUND('',#6041,.T.);
#4971=FACE_OUTER_BOUND('',#6042,.T.);
#4972=FACE_OUTER_BOUND('',#6043,.T.);
#4973=FACE_OUTER_BOUND('',#6044,.T.);
#4974=FACE_OUTER_BOUND('',#6045,.T.);
#4975=FACE_OUTER_BOUND('',#6046,.T.);
#4976=FACE_OUTER_BOUND('',#6047,.T.);
#4977=FACE_OUTER_BOUND('',#6048,.T.);
#4978=FACE_OUTER_BOUND('',#6049,.T.);
#4979=FACE_OUTER_BOUND('',#6050,.T.);
#4980=FACE_OUTER_BOUND('',#6051,.T.);
#4981=FACE_OUTER_BOUND('',#6052,.T.);
#4982=FACE_OUTER_BOUND('',#6053,.T.);
#4983=FACE_OUTER_BOUND('',#6054,.T.);
#4984=FACE_OUTER_BOUND('',#6055,.T.);
#4985=FACE_OUTER_BOUND('',#6056,.T.);
#4986=FACE_OUTER_BOUND('',#6057,.T.);
#4987=FACE_OUTER_BOUND('',#6058,.T.);
#4988=FACE_OUTER_BOUND('',#6059,.T.);
#4989=FACE_OUTER_BOUND('',#6060,.T.);
#4990=FACE_OUTER_BOUND('',#6061,.T.);
#4991=FACE_OUTER_BOUND('',#6062,.T.);
#4992=FACE_OUTER_BOUND('',#6063,.T.);
#4993=FACE_OUTER_BOUND('',#6064,.T.);
#4994=FACE_OUTER_BOUND('',#6065,.T.);
#4995=FACE_OUTER_BOUND('',#6066,.T.);
#4996=FACE_OUTER_BOUND('',#6067,.T.);
#4997=FACE_OUTER_BOUND('',#6068,.T.);
#4998=FACE_OUTER_BOUND('',#6069,.T.);
#4999=FACE_OUTER_BOUND('',#6070,.T.);
#5000=FACE_OUTER_BOUND('',#6071,.T.);
#5001=FACE_OUTER_BOUND('',#6072,.T.);
#5002=FACE_OUTER_BOUND('',#6073,.T.);
#5003=FACE_OUTER_BOUND('',#6074,.T.);
#5004=FACE_OUTER_BOUND('',#6075,.T.);
#5005=FACE_OUTER_BOUND('',#6076,.T.);
#5006=FACE_OUTER_BOUND('',#6077,.T.);
#5007=FACE_OUTER_BOUND('',#6078,.T.);
#5008=FACE_OUTER_BOUND('',#6079,.T.);
#5009=FACE_OUTER_BOUND('',#6080,.T.);
#5010=FACE_OUTER_BOUND('',#6081,.T.);
#5011=FACE_OUTER_BOUND('',#6082,.T.);
#5012=FACE_OUTER_BOUND('',#6083,.T.);
#5013=FACE_OUTER_BOUND('',#6084,.T.);
#5014=FACE_OUTER_BOUND('',#6085,.T.);
#5015=FACE_OUTER_BOUND('',#6086,.T.);
#5016=FACE_OUTER_BOUND('',#6087,.T.);
#5017=FACE_OUTER_BOUND('',#6089,.T.);
#5018=FACE_OUTER_BOUND('',#6091,.T.);
#5019=FACE_OUTER_BOUND('',#6092,.T.);
#5020=FACE_OUTER_BOUND('',#6093,.T.);
#5021=FACE_OUTER_BOUND('',#6094,.T.);
#5022=FACE_OUTER_BOUND('',#6095,.T.);
#5023=FACE_OUTER_BOUND('',#6096,.T.);
#5024=FACE_OUTER_BOUND('',#6097,.T.);
#5025=FACE_OUTER_BOUND('',#6098,.T.);
#5026=FACE_OUTER_BOUND('',#6099,.T.);
#5027=FACE_OUTER_BOUND('',#6100,.T.);
#5028=FACE_OUTER_BOUND('',#6101,.T.);
#5029=FACE_OUTER_BOUND('',#6102,.T.);
#5030=FACE_OUTER_BOUND('',#6103,.T.);
#5031=FACE_OUTER_BOUND('',#6104,.T.);
#5032=FACE_OUTER_BOUND('',#6105,.T.);
#5033=FACE_OUTER_BOUND('',#6106,.T.);
#5034=FACE_OUTER_BOUND('',#6107,.T.);
#5035=FACE_OUTER_BOUND('',#6108,.T.);
#5036=FACE_OUTER_BOUND('',#6109,.T.);
#5037=FACE_OUTER_BOUND('',#6110,.T.);
#5038=FACE_OUTER_BOUND('',#6111,.T.);
#5039=FACE_OUTER_BOUND('',#6116,.T.);
#5040=FACE_OUTER_BOUND('',#6121,.T.);
#5041=FACE_OUTER_BOUND('',#6122,.T.);
#5042=FACE_OUTER_BOUND('',#6123,.T.);
#5043=FACE_OUTER_BOUND('',#6124,.T.);
#5044=FACE_OUTER_BOUND('',#6125,.T.);
#5045=FACE_OUTER_BOUND('',#6126,.T.);
#5046=FACE_OUTER_BOUND('',#6127,.T.);
#5047=FACE_OUTER_BOUND('',#6128,.T.);
#5048=FACE_OUTER_BOUND('',#6129,.T.);
#5049=FACE_OUTER_BOUND('',#6130,.T.);
#5050=FACE_OUTER_BOUND('',#6131,.T.);
#5051=FACE_OUTER_BOUND('',#6132,.T.);
#5052=FACE_OUTER_BOUND('',#6133,.T.);
#5053=FACE_OUTER_BOUND('',#6134,.T.);
#5054=FACE_OUTER_BOUND('',#6135,.T.);
#5055=FACE_OUTER_BOUND('',#6136,.T.);
#5056=FACE_OUTER_BOUND('',#6137,.T.);
#5057=FACE_OUTER_BOUND('',#6138,.T.);
#5058=FACE_OUTER_BOUND('',#6139,.T.);
#5059=FACE_OUTER_BOUND('',#6140,.T.);
#5060=FACE_OUTER_BOUND('',#6141,.T.);
#5061=FACE_OUTER_BOUND('',#6142,.T.);
#5062=FACE_OUTER_BOUND('',#6143,.T.);
#5063=FACE_OUTER_BOUND('',#6144,.T.);
#5064=FACE_OUTER_BOUND('',#6145,.T.);
#5065=FACE_OUTER_BOUND('',#6146,.T.);
#5066=FACE_OUTER_BOUND('',#6147,.T.);
#5067=FACE_OUTER_BOUND('',#6148,.T.);
#5068=FACE_OUTER_BOUND('',#6149,.T.);
#5069=FACE_OUTER_BOUND('',#6150,.T.);
#5070=FACE_OUTER_BOUND('',#6151,.T.);
#5071=FACE_OUTER_BOUND('',#6152,.T.);
#5072=FACE_OUTER_BOUND('',#6169,.T.);
#5073=FACE_OUTER_BOUND('',#6186,.T.);
#5074=FACE_OUTER_BOUND('',#6187,.T.);
#5075=FACE_OUTER_BOUND('',#6188,.T.);
#5076=FACE_OUTER_BOUND('',#6189,.T.);
#5077=FACE_OUTER_BOUND('',#6190,.T.);
#5078=FACE_OUTER_BOUND('',#6191,.T.);
#5079=FACE_OUTER_BOUND('',#6192,.T.);
#5080=FACE_OUTER_BOUND('',#6193,.T.);
#5081=FACE_OUTER_BOUND('',#6194,.T.);
#5082=FACE_OUTER_BOUND('',#6195,.T.);
#5083=FACE_OUTER_BOUND('',#6196,.T.);
#5084=FACE_OUTER_BOUND('',#6197,.T.);
#5085=FACE_OUTER_BOUND('',#6198,.T.);
#5086=FACE_OUTER_BOUND('',#6200,.T.);
#5087=FACE_OUTER_BOUND('',#6202,.T.);
#5088=FACE_OUTER_BOUND('',#6203,.T.);
#5089=FACE_OUTER_BOUND('',#6204,.T.);
#5090=FACE_OUTER_BOUND('',#6206,.T.);
#5091=FACE_OUTER_BOUND('',#6207,.T.);
#5092=FACE_OUTER_BOUND('',#6208,.T.);
#5093=FACE_OUTER_BOUND('',#6209,.T.);
#5094=FACE_OUTER_BOUND('',#6210,.T.);
#5095=FACE_OUTER_BOUND('',#6211,.T.);
#5096=FACE_OUTER_BOUND('',#6212,.T.);
#5097=FACE_OUTER_BOUND('',#6213,.T.);
#5098=FACE_OUTER_BOUND('',#6214,.T.);
#5099=FACE_OUTER_BOUND('',#6215,.T.);
#5100=FACE_OUTER_BOUND('',#6216,.T.);
#5101=FACE_OUTER_BOUND('',#6217,.T.);
#5102=FACE_OUTER_BOUND('',#6218,.T.);
#5103=FACE_OUTER_BOUND('',#6219,.T.);
#5104=FACE_OUTER_BOUND('',#6220,.T.);
#5105=FACE_OUTER_BOUND('',#6221,.T.);
#5106=FACE_OUTER_BOUND('',#6222,.T.);
#5107=FACE_OUTER_BOUND('',#6223,.T.);
#5108=FACE_OUTER_BOUND('',#6224,.T.);
#5109=FACE_OUTER_BOUND('',#6225,.T.);
#5110=FACE_OUTER_BOUND('',#6226,.T.);
#5111=FACE_OUTER_BOUND('',#6227,.T.);
#5112=FACE_OUTER_BOUND('',#6228,.T.);
#5113=FACE_OUTER_BOUND('',#6229,.T.);
#5114=FACE_OUTER_BOUND('',#6230,.T.);
#5115=FACE_OUTER_BOUND('',#6231,.T.);
#5116=FACE_OUTER_BOUND('',#6232,.T.);
#5117=FACE_OUTER_BOUND('',#6233,.T.);
#5118=FACE_OUTER_BOUND('',#6234,.T.);
#5119=FACE_OUTER_BOUND('',#6235,.T.);
#5120=FACE_OUTER_BOUND('',#6236,.T.);
#5121=FACE_OUTER_BOUND('',#6237,.T.);
#5122=FACE_OUTER_BOUND('',#6238,.T.);
#5123=FACE_OUTER_BOUND('',#6239,.T.);
#5124=FACE_OUTER_BOUND('',#6240,.T.);
#5125=FACE_OUTER_BOUND('',#6241,.T.);
#5126=FACE_OUTER_BOUND('',#6242,.T.);
#5127=FACE_OUTER_BOUND('',#6243,.T.);
#5128=FACE_OUTER_BOUND('',#6244,.T.);
#5129=FACE_OUTER_BOUND('',#6245,.T.);
#5130=FACE_OUTER_BOUND('',#6246,.T.);
#5131=FACE_OUTER_BOUND('',#6247,.T.);
#5132=FACE_OUTER_BOUND('',#6249,.T.);
#5133=FACE_OUTER_BOUND('',#6250,.T.);
#5134=FACE_OUTER_BOUND('',#6251,.T.);
#5135=FACE_OUTER_BOUND('',#6252,.T.);
#5136=FACE_OUTER_BOUND('',#6253,.T.);
#5137=FACE_OUTER_BOUND('',#6254,.T.);
#5138=FACE_OUTER_BOUND('',#6255,.T.);
#5139=FACE_OUTER_BOUND('',#6256,.T.);
#5140=FACE_OUTER_BOUND('',#6257,.T.);
#5141=FACE_OUTER_BOUND('',#6258,.T.);
#5142=FACE_OUTER_BOUND('',#6259,.T.);
#5143=FACE_OUTER_BOUND('',#6260,.T.);
#5144=FACE_OUTER_BOUND('',#6261,.T.);
#5145=FACE_OUTER_BOUND('',#6262,.T.);
#5146=FACE_OUTER_BOUND('',#6263,.T.);
#5147=FACE_OUTER_BOUND('',#6264,.T.);
#5148=FACE_OUTER_BOUND('',#6265,.T.);
#5149=FACE_OUTER_BOUND('',#6266,.T.);
#5150=FACE_OUTER_BOUND('',#6267,.T.);
#5151=FACE_OUTER_BOUND('',#6268,.T.);
#5152=FACE_OUTER_BOUND('',#6269,.T.);
#5153=FACE_OUTER_BOUND('',#6270,.T.);
#5154=FACE_OUTER_BOUND('',#6271,.T.);
#5155=FACE_OUTER_BOUND('',#6272,.T.);
#5156=FACE_OUTER_BOUND('',#6273,.T.);
#5157=FACE_OUTER_BOUND('',#6274,.T.);
#5158=FACE_OUTER_BOUND('',#6275,.T.);
#5159=FACE_OUTER_BOUND('',#6276,.T.);
#5160=FACE_OUTER_BOUND('',#6277,.T.);
#5161=FACE_OUTER_BOUND('',#6278,.T.);
#5162=FACE_OUTER_BOUND('',#6279,.T.);
#5163=FACE_OUTER_BOUND('',#6280,.T.);
#5164=FACE_OUTER_BOUND('',#6281,.T.);
#5165=FACE_OUTER_BOUND('',#6282,.T.);
#5166=FACE_OUTER_BOUND('',#6283,.T.);
#5167=FACE_OUTER_BOUND('',#6284,.T.);
#5168=FACE_OUTER_BOUND('',#6285,.T.);
#5169=FACE_OUTER_BOUND('',#6286,.T.);
#5170=FACE_OUTER_BOUND('',#6287,.T.);
#5171=FACE_OUTER_BOUND('',#6288,.T.);
#5172=FACE_OUTER_BOUND('',#6289,.T.);
#5173=FACE_OUTER_BOUND('',#6290,.T.);
#5174=FACE_OUTER_BOUND('',#6291,.T.);
#5175=FACE_OUTER_BOUND('',#6292,.T.);
#5176=FACE_OUTER_BOUND('',#6293,.T.);
#5177=FACE_OUTER_BOUND('',#6294,.T.);
#5178=FACE_OUTER_BOUND('',#6295,.T.);
#5179=FACE_OUTER_BOUND('',#6296,.T.);
#5180=FACE_OUTER_BOUND('',#6297,.T.);
#5181=FACE_OUTER_BOUND('',#6298,.T.);
#5182=FACE_OUTER_BOUND('',#6299,.T.);
#5183=FACE_OUTER_BOUND('',#6300,.T.);
#5184=FACE_OUTER_BOUND('',#6301,.T.);
#5185=FACE_OUTER_BOUND('',#6302,.T.);
#5186=FACE_OUTER_BOUND('',#6303,.T.);
#5187=FACE_OUTER_BOUND('',#6304,.T.);
#5188=FACE_OUTER_BOUND('',#6305,.T.);
#5189=FACE_OUTER_BOUND('',#6306,.T.);
#5190=FACE_OUTER_BOUND('',#6307,.T.);
#5191=FACE_OUTER_BOUND('',#6308,.T.);
#5192=FACE_OUTER_BOUND('',#6309,.T.);
#5193=FACE_OUTER_BOUND('',#6310,.T.);
#5194=FACE_OUTER_BOUND('',#6311,.T.);
#5195=FACE_OUTER_BOUND('',#6312,.T.);
#5196=FACE_OUTER_BOUND('',#6313,.T.);
#5197=FACE_OUTER_BOUND('',#6314,.T.);
#5198=FACE_OUTER_BOUND('',#6315,.T.);
#5199=FACE_OUTER_BOUND('',#6316,.T.);
#5200=FACE_OUTER_BOUND('',#6317,.T.);
#5201=FACE_OUTER_BOUND('',#6318,.T.);
#5202=FACE_OUTER_BOUND('',#6319,.T.);
#5203=FACE_OUTER_BOUND('',#6320,.T.);
#5204=FACE_OUTER_BOUND('',#6321,.T.);
#5205=FACE_OUTER_BOUND('',#6322,.T.);
#5206=FACE_OUTER_BOUND('',#6323,.T.);
#5207=FACE_OUTER_BOUND('',#6324,.T.);
#5208=FACE_OUTER_BOUND('',#6325,.T.);
#5209=FACE_OUTER_BOUND('',#6326,.T.);
#5210=FACE_OUTER_BOUND('',#6327,.T.);
#5211=FACE_OUTER_BOUND('',#6328,.T.);
#5212=FACE_OUTER_BOUND('',#6329,.T.);
#5213=FACE_OUTER_BOUND('',#6330,.T.);
#5214=FACE_OUTER_BOUND('',#6331,.T.);
#5215=FACE_OUTER_BOUND('',#6332,.T.);
#5216=FACE_OUTER_BOUND('',#6333,.T.);
#5217=FACE_OUTER_BOUND('',#6334,.T.);
#5218=FACE_OUTER_BOUND('',#6335,.T.);
#5219=FACE_OUTER_BOUND('',#6336,.T.);
#5220=FACE_OUTER_BOUND('',#6337,.T.);
#5221=FACE_OUTER_BOUND('',#6338,.T.);
#5222=FACE_OUTER_BOUND('',#6339,.T.);
#5223=FACE_OUTER_BOUND('',#6340,.T.);
#5224=FACE_OUTER_BOUND('',#6341,.T.);
#5225=FACE_OUTER_BOUND('',#6342,.T.);
#5226=FACE_OUTER_BOUND('',#6343,.T.);
#5227=FACE_OUTER_BOUND('',#6344,.T.);
#5228=FACE_OUTER_BOUND('',#6345,.T.);
#5229=FACE_OUTER_BOUND('',#6346,.T.);
#5230=FACE_OUTER_BOUND('',#6347,.T.);
#5231=FACE_OUTER_BOUND('',#6348,.T.);
#5232=FACE_OUTER_BOUND('',#6349,.T.);
#5233=FACE_OUTER_BOUND('',#6350,.T.);
#5234=FACE_OUTER_BOUND('',#6351,.T.);
#5235=FACE_OUTER_BOUND('',#6352,.T.);
#5236=FACE_OUTER_BOUND('',#6353,.T.);
#5237=FACE_OUTER_BOUND('',#6354,.T.);
#5238=FACE_OUTER_BOUND('',#6355,.T.);
#5239=FACE_OUTER_BOUND('',#6356,.T.);
#5240=FACE_OUTER_BOUND('',#6357,.T.);
#5241=FACE_OUTER_BOUND('',#6358,.T.);
#5242=FACE_OUTER_BOUND('',#6359,.T.);
#5243=FACE_OUTER_BOUND('',#6360,.T.);
#5244=FACE_OUTER_BOUND('',#6361,.T.);
#5245=FACE_OUTER_BOUND('',#6362,.T.);
#5246=FACE_OUTER_BOUND('',#6363,.T.);
#5247=FACE_OUTER_BOUND('',#6365,.T.);
#5248=FACE_OUTER_BOUND('',#6366,.T.);
#5249=FACE_OUTER_BOUND('',#6368,.T.);
#5250=FACE_OUTER_BOUND('',#6370,.T.);
#5251=FACE_OUTER_BOUND('',#6371,.T.);
#5252=FACE_OUTER_BOUND('',#6373,.T.);
#5253=FACE_OUTER_BOUND('',#6374,.T.);
#5254=FACE_OUTER_BOUND('',#6375,.T.);
#5255=FACE_OUTER_BOUND('',#6376,.T.);
#5256=FACE_OUTER_BOUND('',#6377,.T.);
#5257=FACE_OUTER_BOUND('',#6378,.T.);
#5258=FACE_OUTER_BOUND('',#6379,.T.);
#5259=FACE_OUTER_BOUND('',#6380,.T.);
#5260=FACE_OUTER_BOUND('',#6381,.T.);
#5261=FACE_OUTER_BOUND('',#6382,.T.);
#5262=FACE_OUTER_BOUND('',#6383,.T.);
#5263=FACE_OUTER_BOUND('',#6384,.T.);
#5264=FACE_OUTER_BOUND('',#6385,.T.);
#5265=FACE_OUTER_BOUND('',#6387,.T.);
#5266=FACE_OUTER_BOUND('',#6389,.T.);
#5267=FACE_OUTER_BOUND('',#6391,.T.);
#5268=FACE_OUTER_BOUND('',#6393,.T.);
#5269=FACE_OUTER_BOUND('',#6394,.T.);
#5270=FACE_OUTER_BOUND('',#6395,.T.);
#5271=FACE_OUTER_BOUND('',#6396,.T.);
#5272=FACE_OUTER_BOUND('',#6397,.T.);
#5273=FACE_OUTER_BOUND('',#6398,.T.);
#5274=FACE_OUTER_BOUND('',#6399,.T.);
#5275=FACE_OUTER_BOUND('',#6400,.T.);
#5276=FACE_OUTER_BOUND('',#6401,.T.);
#5277=FACE_OUTER_BOUND('',#6402,.T.);
#5278=FACE_OUTER_BOUND('',#6403,.T.);
#5279=FACE_OUTER_BOUND('',#6404,.T.);
#5280=FACE_OUTER_BOUND('',#6405,.T.);
#5281=FACE_OUTER_BOUND('',#6406,.T.);
#5282=FACE_OUTER_BOUND('',#6407,.T.);
#5283=FACE_OUTER_BOUND('',#6408,.T.);
#5284=FACE_OUTER_BOUND('',#6409,.T.);
#5285=FACE_OUTER_BOUND('',#6410,.T.);
#5286=FACE_OUTER_BOUND('',#6411,.T.);
#5287=FACE_OUTER_BOUND('',#6412,.T.);
#5288=FACE_OUTER_BOUND('',#6413,.T.);
#5289=FACE_OUTER_BOUND('',#6414,.T.);
#5290=FACE_OUTER_BOUND('',#6415,.T.);
#5291=FACE_OUTER_BOUND('',#6416,.T.);
#5292=FACE_OUTER_BOUND('',#6417,.T.);
#5293=FACE_OUTER_BOUND('',#6418,.T.);
#5294=FACE_OUTER_BOUND('',#6419,.T.);
#5295=FACE_OUTER_BOUND('',#6420,.T.);
#5296=FACE_OUTER_BOUND('',#6421,.T.);
#5297=FACE_OUTER_BOUND('',#6422,.T.);
#5298=FACE_OUTER_BOUND('',#6423,.T.);
#5299=FACE_OUTER_BOUND('',#6424,.T.);
#5300=FACE_OUTER_BOUND('',#6425,.T.);
#5301=FACE_OUTER_BOUND('',#6426,.T.);
#5302=FACE_OUTER_BOUND('',#6427,.T.);
#5303=FACE_OUTER_BOUND('',#6428,.T.);
#5304=FACE_OUTER_BOUND('',#6429,.T.);
#5305=FACE_OUTER_BOUND('',#6430,.T.);
#5306=FACE_OUTER_BOUND('',#6431,.T.);
#5307=FACE_OUTER_BOUND('',#6432,.T.);
#5308=FACE_OUTER_BOUND('',#6433,.T.);
#5309=FACE_OUTER_BOUND('',#6434,.T.);
#5310=FACE_OUTER_BOUND('',#6435,.T.);
#5311=FACE_OUTER_BOUND('',#6436,.T.);
#5312=FACE_OUTER_BOUND('',#6437,.T.);
#5313=FACE_OUTER_BOUND('',#6438,.T.);
#5314=FACE_OUTER_BOUND('',#6439,.T.);
#5315=FACE_OUTER_BOUND('',#6440,.T.);
#5316=FACE_OUTER_BOUND('',#6441,.T.);
#5317=FACE_OUTER_BOUND('',#6442,.T.);
#5318=FACE_OUTER_BOUND('',#6443,.T.);
#5319=FACE_OUTER_BOUND('',#6444,.T.);
#5320=FACE_OUTER_BOUND('',#6445,.T.);
#5321=FACE_OUTER_BOUND('',#6446,.T.);
#5322=FACE_OUTER_BOUND('',#6447,.T.);
#5323=FACE_OUTER_BOUND('',#6448,.T.);
#5324=FACE_OUTER_BOUND('',#6449,.T.);
#5325=FACE_OUTER_BOUND('',#6450,.T.);
#5326=FACE_OUTER_BOUND('',#6451,.T.);
#5327=FACE_OUTER_BOUND('',#6452,.T.);
#5328=FACE_OUTER_BOUND('',#6453,.T.);
#5329=FACE_OUTER_BOUND('',#6454,.T.);
#5330=FACE_OUTER_BOUND('',#6455,.T.);
#5331=FACE_OUTER_BOUND('',#6456,.T.);
#5332=FACE_OUTER_BOUND('',#6457,.T.);
#5333=FACE_OUTER_BOUND('',#6458,.T.);
#5334=FACE_OUTER_BOUND('',#6459,.T.);
#5335=FACE_OUTER_BOUND('',#6460,.T.);
#5336=FACE_OUTER_BOUND('',#6461,.T.);
#5337=FACE_OUTER_BOUND('',#6462,.T.);
#5338=FACE_OUTER_BOUND('',#6463,.T.);
#5339=FACE_OUTER_BOUND('',#6464,.T.);
#5340=FACE_OUTER_BOUND('',#6465,.T.);
#5341=FACE_OUTER_BOUND('',#6467,.T.);
#5342=FACE_OUTER_BOUND('',#6468,.T.);
#5343=FACE_OUTER_BOUND('',#6469,.T.);
#5344=FACE_OUTER_BOUND('',#6470,.T.);
#5345=FACE_OUTER_BOUND('',#6471,.T.);
#5346=FACE_OUTER_BOUND('',#6472,.T.);
#5347=FACE_OUTER_BOUND('',#6473,.T.);
#5348=FACE_OUTER_BOUND('',#6474,.T.);
#5349=FACE_OUTER_BOUND('',#6475,.T.);
#5350=FACE_OUTER_BOUND('',#6476,.T.);
#5351=FACE_OUTER_BOUND('',#6477,.T.);
#5352=FACE_OUTER_BOUND('',#6478,.T.);
#5353=FACE_OUTER_BOUND('',#6479,.T.);
#5354=FACE_OUTER_BOUND('',#6480,.T.);
#5355=FACE_OUTER_BOUND('',#6481,.T.);
#5356=FACE_OUTER_BOUND('',#6482,.T.);
#5357=FACE_OUTER_BOUND('',#6483,.T.);
#5358=FACE_OUTER_BOUND('',#6486,.T.);
#5359=FACE_OUTER_BOUND('',#6487,.T.);
#5360=FACE_OUTER_BOUND('',#6488,.T.);
#5361=FACE_OUTER_BOUND('',#6489,.T.);
#5362=FACE_OUTER_BOUND('',#6490,.T.);
#5363=FACE_OUTER_BOUND('',#6491,.T.);
#5364=FACE_OUTER_BOUND('',#6492,.T.);
#5365=FACE_OUTER_BOUND('',#6493,.T.);
#5366=FACE_OUTER_BOUND('',#6494,.T.);
#5367=FACE_OUTER_BOUND('',#6495,.T.);
#5368=FACE_OUTER_BOUND('',#6496,.T.);
#5369=FACE_OUTER_BOUND('',#6497,.T.);
#5370=FACE_OUTER_BOUND('',#6498,.T.);
#5371=FACE_OUTER_BOUND('',#6499,.T.);
#5372=FACE_OUTER_BOUND('',#6500,.T.);
#5373=FACE_OUTER_BOUND('',#6501,.T.);
#5374=FACE_OUTER_BOUND('',#6502,.T.);
#5375=FACE_OUTER_BOUND('',#6503,.T.);
#5376=FACE_OUTER_BOUND('',#6504,.T.);
#5377=FACE_OUTER_BOUND('',#6506,.T.);
#5378=FACE_OUTER_BOUND('',#6507,.T.);
#5379=FACE_OUTER_BOUND('',#6508,.T.);
#5380=FACE_OUTER_BOUND('',#6509,.T.);
#5381=FACE_OUTER_BOUND('',#6510,.T.);
#5382=FACE_OUTER_BOUND('',#6511,.T.);
#5383=FACE_OUTER_BOUND('',#6512,.T.);
#5384=FACE_OUTER_BOUND('',#6513,.T.);
#5385=FACE_OUTER_BOUND('',#6514,.T.);
#5386=FACE_OUTER_BOUND('',#6515,.T.);
#5387=FACE_OUTER_BOUND('',#6516,.T.);
#5388=FACE_OUTER_BOUND('',#6517,.T.);
#5389=FACE_OUTER_BOUND('',#6518,.T.);
#5390=FACE_OUTER_BOUND('',#6519,.T.);
#5391=FACE_OUTER_BOUND('',#6520,.T.);
#5392=FACE_OUTER_BOUND('',#6521,.T.);
#5393=FACE_OUTER_BOUND('',#6522,.T.);
#5394=FACE_OUTER_BOUND('',#6523,.T.);
#5395=FACE_OUTER_BOUND('',#6524,.T.);
#5396=FACE_OUTER_BOUND('',#6525,.T.);
#5397=FACE_OUTER_BOUND('',#6526,.T.);
#5398=FACE_OUTER_BOUND('',#6527,.T.);
#5399=FACE_OUTER_BOUND('',#6528,.T.);
#5400=FACE_OUTER_BOUND('',#6529,.T.);
#5401=FACE_OUTER_BOUND('',#6530,.T.);
#5402=FACE_OUTER_BOUND('',#6531,.T.);
#5403=FACE_OUTER_BOUND('',#6532,.T.);
#5404=FACE_OUTER_BOUND('',#6533,.T.);
#5405=FACE_OUTER_BOUND('',#6534,.T.);
#5406=FACE_OUTER_BOUND('',#6535,.T.);
#5407=FACE_OUTER_BOUND('',#6536,.T.);
#5408=FACE_OUTER_BOUND('',#6537,.T.);
#5409=FACE_OUTER_BOUND('',#6538,.T.);
#5410=FACE_OUTER_BOUND('',#6539,.T.);
#5411=FACE_OUTER_BOUND('',#6540,.T.);
#5412=FACE_OUTER_BOUND('',#6541,.T.);
#5413=FACE_OUTER_BOUND('',#6542,.T.);
#5414=FACE_OUTER_BOUND('',#6543,.T.);
#5415=FACE_OUTER_BOUND('',#6544,.T.);
#5416=FACE_OUTER_BOUND('',#6545,.T.);
#5417=FACE_OUTER_BOUND('',#6546,.T.);
#5418=FACE_OUTER_BOUND('',#6547,.T.);
#5419=FACE_OUTER_BOUND('',#6548,.T.);
#5420=FACE_OUTER_BOUND('',#6549,.T.);
#5421=FACE_OUTER_BOUND('',#6551,.T.);
#5422=FACE_OUTER_BOUND('',#6552,.T.);
#5423=FACE_OUTER_BOUND('',#6553,.T.);
#5424=FACE_OUTER_BOUND('',#6554,.T.);
#5425=FACE_OUTER_BOUND('',#6555,.T.);
#5426=FACE_OUTER_BOUND('',#6556,.T.);
#5427=FACE_OUTER_BOUND('',#6558,.T.);
#5428=FACE_OUTER_BOUND('',#6559,.T.);
#5429=FACE_OUTER_BOUND('',#6561,.T.);
#5430=FACE_OUTER_BOUND('',#6563,.T.);
#5431=FACE_OUTER_BOUND('',#6564,.T.);
#5432=FACE_OUTER_BOUND('',#6565,.T.);
#5433=FACE_OUTER_BOUND('',#6566,.T.);
#5434=FACE_OUTER_BOUND('',#6567,.T.);
#5435=FACE_OUTER_BOUND('',#6568,.T.);
#5436=FACE_OUTER_BOUND('',#6570,.T.);
#5437=FACE_OUTER_BOUND('',#6571,.T.);
#5438=FACE_OUTER_BOUND('',#6572,.T.);
#5439=FACE_OUTER_BOUND('',#6573,.T.);
#5440=FACE_OUTER_BOUND('',#6574,.T.);
#5441=FACE_OUTER_BOUND('',#6575,.T.);
#5442=FACE_OUTER_BOUND('',#6576,.T.);
#5443=FACE_OUTER_BOUND('',#6577,.T.);
#5444=FACE_OUTER_BOUND('',#6578,.T.);
#5445=FACE_OUTER_BOUND('',#6580,.T.);
#5446=FACE_OUTER_BOUND('',#6581,.T.);
#5447=FACE_OUTER_BOUND('',#6582,.T.);
#5448=FACE_OUTER_BOUND('',#6583,.T.);
#5449=FACE_OUTER_BOUND('',#6584,.T.);
#5450=FACE_OUTER_BOUND('',#6586,.T.);
#5451=FACE_OUTER_BOUND('',#6587,.T.);
#5452=FACE_OUTER_BOUND('',#6589,.T.);
#5453=FACE_OUTER_BOUND('',#6590,.T.);
#5454=FACE_OUTER_BOUND('',#6591,.T.);
#5455=FACE_OUTER_BOUND('',#6592,.T.);
#5456=FACE_OUTER_BOUND('',#6593,.T.);
#5457=FACE_OUTER_BOUND('',#6595,.T.);
#5458=FACE_OUTER_BOUND('',#6597,.T.);
#5459=FACE_OUTER_BOUND('',#6598,.T.);
#5460=FACE_OUTER_BOUND('',#6599,.T.);
#5461=FACE_OUTER_BOUND('',#6600,.T.);
#5462=FACE_OUTER_BOUND('',#6601,.T.);
#5463=FACE_OUTER_BOUND('',#6602,.T.);
#5464=FACE_OUTER_BOUND('',#6603,.T.);
#5465=FACE_OUTER_BOUND('',#6604,.T.);
#5466=FACE_OUTER_BOUND('',#6605,.T.);
#5467=FACE_OUTER_BOUND('',#6607,.T.);
#5468=FACE_OUTER_BOUND('',#6608,.T.);
#5469=FACE_OUTER_BOUND('',#6609,.T.);
#5470=FACE_OUTER_BOUND('',#6610,.T.);
#5471=FACE_OUTER_BOUND('',#6611,.T.);
#5472=FACE_OUTER_BOUND('',#6612,.T.);
#5473=FACE_OUTER_BOUND('',#6613,.T.);
#5474=FACE_OUTER_BOUND('',#6614,.T.);
#5475=FACE_OUTER_BOUND('',#6615,.T.);
#5476=FACE_OUTER_BOUND('',#6617,.T.);
#5477=FACE_OUTER_BOUND('',#6618,.T.);
#5478=FACE_OUTER_BOUND('',#6619,.T.);
#5479=FACE_OUTER_BOUND('',#6620,.T.);
#5480=FACE_OUTER_BOUND('',#6621,.T.);
#5481=FACE_OUTER_BOUND('',#6622,.T.);
#5482=FACE_OUTER_BOUND('',#6623,.T.);
#5483=FACE_OUTER_BOUND('',#6624,.T.);
#5484=FACE_OUTER_BOUND('',#6625,.T.);
#5485=FACE_OUTER_BOUND('',#6627,.T.);
#5486=FACE_OUTER_BOUND('',#6628,.T.);
#5487=FACE_OUTER_BOUND('',#6629,.T.);
#5488=FACE_OUTER_BOUND('',#6630,.T.);
#5489=FACE_OUTER_BOUND('',#6631,.T.);
#5490=FACE_OUTER_BOUND('',#6632,.T.);
#5491=FACE_OUTER_BOUND('',#6633,.T.);
#5492=FACE_OUTER_BOUND('',#6634,.T.);
#5493=FACE_OUTER_BOUND('',#6635,.T.);
#5494=FACE_OUTER_BOUND('',#6636,.T.);
#5495=FACE_OUTER_BOUND('',#6637,.T.);
#5496=FACE_OUTER_BOUND('',#6638,.T.);
#5497=FACE_OUTER_BOUND('',#6639,.T.);
#5498=FACE_OUTER_BOUND('',#6640,.T.);
#5499=FACE_OUTER_BOUND('',#6641,.T.);
#5500=FACE_OUTER_BOUND('',#6643,.T.);
#5501=FACE_OUTER_BOUND('',#6645,.T.);
#5502=FACE_OUTER_BOUND('',#6646,.T.);
#5503=FACE_OUTER_BOUND('',#6647,.T.);
#5504=FACE_OUTER_BOUND('',#6648,.T.);
#5505=FACE_OUTER_BOUND('',#6649,.T.);
#5506=FACE_OUTER_BOUND('',#6650,.T.);
#5507=FACE_OUTER_BOUND('',#6651,.T.);
#5508=FACE_OUTER_BOUND('',#6652,.T.);
#5509=FACE_OUTER_BOUND('',#6653,.T.);
#5510=FACE_OUTER_BOUND('',#6654,.T.);
#5511=FACE_OUTER_BOUND('',#6655,.T.);
#5512=FACE_OUTER_BOUND('',#6656,.T.);
#5513=FACE_OUTER_BOUND('',#6657,.T.);
#5514=FACE_OUTER_BOUND('',#6658,.T.);
#5515=FACE_OUTER_BOUND('',#6659,.T.);
#5516=FACE_OUTER_BOUND('',#6660,.T.);
#5517=FACE_OUTER_BOUND('',#6661,.T.);
#5518=FACE_OUTER_BOUND('',#6662,.T.);
#5519=FACE_OUTER_BOUND('',#6663,.T.);
#5520=FACE_OUTER_BOUND('',#6664,.T.);
#5521=FACE_OUTER_BOUND('',#6665,.T.);
#5522=FACE_OUTER_BOUND('',#6666,.T.);
#5523=FACE_OUTER_BOUND('',#6667,.T.);
#5524=FACE_OUTER_BOUND('',#6668,.T.);
#5525=FACE_OUTER_BOUND('',#6669,.T.);
#5526=FACE_OUTER_BOUND('',#6671,.T.);
#5527=FACE_OUTER_BOUND('',#6672,.T.);
#5528=FACE_OUTER_BOUND('',#6673,.T.);
#5529=FACE_OUTER_BOUND('',#6674,.T.);
#5530=FACE_OUTER_BOUND('',#6675,.T.);
#5531=FACE_OUTER_BOUND('',#6676,.T.);
#5532=FACE_OUTER_BOUND('',#6677,.T.);
#5533=FACE_OUTER_BOUND('',#6678,.T.);
#5534=FACE_OUTER_BOUND('',#6679,.T.);
#5535=FACE_OUTER_BOUND('',#6680,.T.);
#5536=FACE_OUTER_BOUND('',#6681,.T.);
#5537=FACE_OUTER_BOUND('',#6682,.T.);
#5538=FACE_OUTER_BOUND('',#6683,.T.);
#5539=FACE_OUTER_BOUND('',#6684,.T.);
#5540=FACE_OUTER_BOUND('',#6685,.T.);
#5541=FACE_OUTER_BOUND('',#6686,.T.);
#5542=FACE_OUTER_BOUND('',#6687,.T.);
#5543=FACE_OUTER_BOUND('',#6689,.T.);
#5544=FACE_OUTER_BOUND('',#6690,.T.);
#5545=FACE_OUTER_BOUND('',#6691,.T.);
#5546=FACE_OUTER_BOUND('',#6693,.T.);
#5547=FACE_OUTER_BOUND('',#6694,.T.);
#5548=FACE_OUTER_BOUND('',#6695,.T.);
#5549=FACE_OUTER_BOUND('',#6696,.T.);
#5550=FACE_OUTER_BOUND('',#6697,.T.);
#5551=FACE_OUTER_BOUND('',#6698,.T.);
#5552=FACE_OUTER_BOUND('',#6699,.T.);
#5553=FACE_OUTER_BOUND('',#6700,.T.);
#5554=FACE_OUTER_BOUND('',#6701,.T.);
#5555=FACE_OUTER_BOUND('',#6702,.T.);
#5556=FACE_OUTER_BOUND('',#6703,.T.);
#5557=FACE_OUTER_BOUND('',#6705,.T.);
#5558=FACE_OUTER_BOUND('',#6707,.T.);
#5559=FACE_OUTER_BOUND('',#6709,.T.);
#5560=FACE_OUTER_BOUND('',#6711,.T.);
#5561=FACE_OUTER_BOUND('',#6713,.T.);
#5562=FACE_OUTER_BOUND('',#6714,.T.);
#5563=FACE_OUTER_BOUND('',#6715,.T.);
#5564=FACE_OUTER_BOUND('',#6716,.T.);
#5565=FACE_OUTER_BOUND('',#6717,.T.);
#5566=FACE_OUTER_BOUND('',#6718,.T.);
#5567=FACE_OUTER_BOUND('',#6719,.T.);
#5568=FACE_OUTER_BOUND('',#6720,.T.);
#5569=FACE_OUTER_BOUND('',#6721,.T.);
#5570=FACE_OUTER_BOUND('',#6722,.T.);
#5571=FACE_OUTER_BOUND('',#6723,.T.);
#5572=FACE_OUTER_BOUND('',#6724,.T.);
#5573=FACE_OUTER_BOUND('',#6725,.T.);
#5574=FACE_OUTER_BOUND('',#6726,.T.);
#5575=FACE_OUTER_BOUND('',#6727,.T.);
#5576=FACE_OUTER_BOUND('',#6728,.T.);
#5577=FACE_OUTER_BOUND('',#6729,.T.);
#5578=FACE_OUTER_BOUND('',#6730,.T.);
#5579=FACE_OUTER_BOUND('',#6731,.T.);
#5580=FACE_OUTER_BOUND('',#6732,.T.);
#5581=FACE_OUTER_BOUND('',#6733,.T.);
#5582=FACE_OUTER_BOUND('',#6734,.T.);
#5583=FACE_OUTER_BOUND('',#6735,.T.);
#5584=FACE_OUTER_BOUND('',#6736,.T.);
#5585=FACE_OUTER_BOUND('',#6737,.T.);
#5586=FACE_OUTER_BOUND('',#6738,.T.);
#5587=FACE_OUTER_BOUND('',#6739,.T.);
#5588=FACE_OUTER_BOUND('',#6741,.T.);
#5589=FACE_OUTER_BOUND('',#6742,.T.);
#5590=FACE_OUTER_BOUND('',#6743,.T.);
#5591=FACE_OUTER_BOUND('',#6744,.T.);
#5592=FACE_OUTER_BOUND('',#6745,.T.);
#5593=FACE_OUTER_BOUND('',#6746,.T.);
#5594=FACE_OUTER_BOUND('',#6747,.T.);
#5595=FACE_OUTER_BOUND('',#6749,.T.);
#5596=FACE_OUTER_BOUND('',#6750,.T.);
#5597=FACE_OUTER_BOUND('',#6751,.T.);
#5598=FACE_OUTER_BOUND('',#6752,.T.);
#5599=FACE_OUTER_BOUND('',#6753,.T.);
#5600=FACE_OUTER_BOUND('',#6754,.T.);
#5601=FACE_OUTER_BOUND('',#6755,.T.);
#5602=FACE_OUTER_BOUND('',#6756,.T.);
#5603=FACE_OUTER_BOUND('',#6757,.T.);
#5604=FACE_OUTER_BOUND('',#6758,.T.);
#5605=FACE_OUTER_BOUND('',#6759,.T.);
#5606=FACE_OUTER_BOUND('',#6760,.T.);
#5607=FACE_OUTER_BOUND('',#6761,.T.);
#5608=FACE_OUTER_BOUND('',#6762,.T.);
#5609=FACE_OUTER_BOUND('',#6763,.T.);
#5610=FACE_OUTER_BOUND('',#6764,.T.);
#5611=FACE_OUTER_BOUND('',#6765,.T.);
#5612=FACE_OUTER_BOUND('',#6766,.T.);
#5613=FACE_OUTER_BOUND('',#6767,.T.);
#5614=FACE_OUTER_BOUND('',#6768,.T.);
#5615=FACE_OUTER_BOUND('',#6769,.T.);
#5616=FACE_OUTER_BOUND('',#6770,.T.);
#5617=FACE_OUTER_BOUND('',#6771,.T.);
#5618=FACE_OUTER_BOUND('',#6772,.T.);
#5619=FACE_OUTER_BOUND('',#6773,.T.);
#5620=FACE_OUTER_BOUND('',#6774,.T.);
#5621=FACE_OUTER_BOUND('',#6775,.T.);
#5622=FACE_OUTER_BOUND('',#6776,.T.);
#5623=FACE_OUTER_BOUND('',#6777,.T.);
#5624=FACE_OUTER_BOUND('',#6778,.T.);
#5625=FACE_OUTER_BOUND('',#6779,.T.);
#5626=FACE_OUTER_BOUND('',#6780,.T.);
#5627=FACE_OUTER_BOUND('',#6782,.T.);
#5628=FACE_OUTER_BOUND('',#6783,.T.);
#5629=FACE_OUTER_BOUND('',#6784,.T.);
#5630=FACE_OUTER_BOUND('',#6785,.T.);
#5631=FACE_OUTER_BOUND('',#6786,.T.);
#5632=FACE_OUTER_BOUND('',#6787,.T.);
#5633=FACE_OUTER_BOUND('',#6788,.T.);
#5634=FACE_OUTER_BOUND('',#6789,.T.);
#5635=FACE_OUTER_BOUND('',#6790,.T.);
#5636=FACE_OUTER_BOUND('',#6791,.T.);
#5637=FACE_OUTER_BOUND('',#6792,.T.);
#5638=FACE_OUTER_BOUND('',#6793,.T.);
#5639=FACE_OUTER_BOUND('',#6794,.T.);
#5640=FACE_OUTER_BOUND('',#6795,.T.);
#5641=FACE_OUTER_BOUND('',#6796,.T.);
#5642=FACE_OUTER_BOUND('',#6797,.T.);
#5643=FACE_OUTER_BOUND('',#6798,.T.);
#5644=FACE_OUTER_BOUND('',#6799,.T.);
#5645=FACE_OUTER_BOUND('',#6800,.T.);
#5646=FACE_OUTER_BOUND('',#6801,.T.);
#5647=FACE_OUTER_BOUND('',#6802,.T.);
#5648=FACE_OUTER_BOUND('',#6803,.T.);
#5649=FACE_OUTER_BOUND('',#6804,.T.);
#5650=FACE_OUTER_BOUND('',#6805,.T.);
#5651=FACE_OUTER_BOUND('',#6806,.T.);
#5652=FACE_OUTER_BOUND('',#6807,.T.);
#5653=FACE_OUTER_BOUND('',#6808,.T.);
#5654=FACE_OUTER_BOUND('',#6809,.T.);
#5655=FACE_OUTER_BOUND('',#6810,.T.);
#5656=FACE_OUTER_BOUND('',#6811,.T.);
#5657=FACE_OUTER_BOUND('',#6812,.T.);
#5658=FACE_OUTER_BOUND('',#6813,.T.);
#5659=FACE_OUTER_BOUND('',#6814,.T.);
#5660=FACE_OUTER_BOUND('',#6815,.T.);
#5661=FACE_OUTER_BOUND('',#6816,.T.);
#5662=FACE_OUTER_BOUND('',#6817,.T.);
#5663=FACE_OUTER_BOUND('',#6819,.T.);
#5664=FACE_OUTER_BOUND('',#6820,.T.);
#5665=FACE_OUTER_BOUND('',#6826,.T.);
#5666=FACE_OUTER_BOUND('',#6827,.T.);
#5667=FACE_OUTER_BOUND('',#6828,.T.);
#5668=FACE_OUTER_BOUND('',#6829,.T.);
#5669=FACE_OUTER_BOUND('',#6830,.T.);
#5670=FACE_OUTER_BOUND('',#6831,.T.);
#5671=FACE_OUTER_BOUND('',#6832,.T.);
#5672=FACE_OUTER_BOUND('',#6833,.T.);
#5673=FACE_OUTER_BOUND('',#6834,.T.);
#5674=FACE_OUTER_BOUND('',#6835,.T.);
#5675=FACE_OUTER_BOUND('',#6836,.T.);
#5676=FACE_OUTER_BOUND('',#6837,.T.);
#5677=FACE_OUTER_BOUND('',#6838,.T.);
#5678=FACE_OUTER_BOUND('',#6839,.T.);
#5679=FACE_OUTER_BOUND('',#6840,.T.);
#5680=FACE_OUTER_BOUND('',#6841,.T.);
#5681=FACE_OUTER_BOUND('',#6842,.T.);
#5682=FACE_OUTER_BOUND('',#6844,.T.);
#5683=FACE_OUTER_BOUND('',#6845,.T.);
#5684=FACE_OUTER_BOUND('',#6847,.T.);
#5685=FACE_OUTER_BOUND('',#6848,.T.);
#5686=FACE_OUTER_BOUND('',#6850,.T.);
#5687=FACE_OUTER_BOUND('',#6851,.T.);
#5688=FACE_OUTER_BOUND('',#6852,.T.);
#5689=FACE_OUTER_BOUND('',#6853,.T.);
#5690=FACE_OUTER_BOUND('',#6854,.T.);
#5691=FACE_OUTER_BOUND('',#6855,.T.);
#5692=FACE_OUTER_BOUND('',#6856,.T.);
#5693=FACE_OUTER_BOUND('',#6858,.T.);
#5694=FACE_OUTER_BOUND('',#6859,.T.);
#5695=FACE_OUTER_BOUND('',#6861,.T.);
#5696=FACE_OUTER_BOUND('',#6863,.T.);
#5697=FACE_OUTER_BOUND('',#6864,.T.);
#5698=FACE_OUTER_BOUND('',#6865,.T.);
#5699=FACE_OUTER_BOUND('',#6866,.T.);
#5700=FACE_OUTER_BOUND('',#6867,.T.);
#5701=FACE_OUTER_BOUND('',#6868,.T.);
#5702=FACE_OUTER_BOUND('',#6869,.T.);
#5703=FACE_OUTER_BOUND('',#6870,.T.);
#5704=FACE_OUTER_BOUND('',#6871,.T.);
#5705=FACE_OUTER_BOUND('',#6872,.T.);
#5706=FACE_OUTER_BOUND('',#6873,.T.);
#5707=FACE_OUTER_BOUND('',#6874,.T.);
#5708=FACE_OUTER_BOUND('',#6875,.T.);
#5709=FACE_OUTER_BOUND('',#6876,.T.);
#5710=FACE_OUTER_BOUND('',#6878,.T.);
#5711=FACE_OUTER_BOUND('',#6879,.T.);
#5712=FACE_OUTER_BOUND('',#6880,.T.);
#5713=FACE_OUTER_BOUND('',#6881,.T.);
#5714=FACE_OUTER_BOUND('',#6882,.T.);
#5715=FACE_OUTER_BOUND('',#6883,.T.);
#5716=FACE_OUTER_BOUND('',#6884,.T.);
#5717=FACE_OUTER_BOUND('',#6885,.T.);
#5718=FACE_OUTER_BOUND('',#6886,.T.);
#5719=FACE_OUTER_BOUND('',#6887,.T.);
#5720=FACE_OUTER_BOUND('',#6888,.T.);
#5721=FACE_OUTER_BOUND('',#6889,.T.);
#5722=FACE_OUTER_BOUND('',#6890,.T.);
#5723=FACE_OUTER_BOUND('',#6891,.T.);
#5724=FACE_OUTER_BOUND('',#6892,.T.);
#5725=FACE_OUTER_BOUND('',#6893,.T.);
#5726=FACE_OUTER_BOUND('',#6895,.T.);
#5727=FACE_OUTER_BOUND('',#6896,.T.);
#5728=FACE_OUTER_BOUND('',#6897,.T.);
#5729=FACE_OUTER_BOUND('',#6899,.T.);
#5730=FACE_OUTER_BOUND('',#6900,.T.);
#5731=FACE_OUTER_BOUND('',#6901,.T.);
#5732=FACE_OUTER_BOUND('',#6902,.T.);
#5733=FACE_OUTER_BOUND('',#6903,.T.);
#5734=FACE_OUTER_BOUND('',#6904,.T.);
#5735=FACE_OUTER_BOUND('',#6905,.T.);
#5736=FACE_OUTER_BOUND('',#6907,.T.);
#5737=FACE_OUTER_BOUND('',#6908,.T.);
#5738=FACE_OUTER_BOUND('',#6909,.T.);
#5739=FACE_OUTER_BOUND('',#6910,.T.);
#5740=FACE_OUTER_BOUND('',#6911,.T.);
#5741=FACE_OUTER_BOUND('',#6912,.T.);
#5742=FACE_OUTER_BOUND('',#6913,.T.);
#5743=FACE_OUTER_BOUND('',#6914,.T.);
#5744=FACE_OUTER_BOUND('',#6915,.T.);
#5745=FACE_OUTER_BOUND('',#6916,.T.);
#5746=FACE_OUTER_BOUND('',#6917,.T.);
#5747=FACE_OUTER_BOUND('',#6918,.T.);
#5748=FACE_OUTER_BOUND('',#6919,.T.);
#5749=FACE_OUTER_BOUND('',#6920,.T.);
#5750=FACE_OUTER_BOUND('',#6921,.T.);
#5751=FACE_OUTER_BOUND('',#6922,.T.);
#5752=FACE_OUTER_BOUND('',#6923,.T.);
#5753=FACE_OUTER_BOUND('',#6924,.T.);
#5754=FACE_OUTER_BOUND('',#6925,.T.);
#5755=FACE_OUTER_BOUND('',#6926,.T.);
#5756=FACE_OUTER_BOUND('',#6927,.T.);
#5757=FACE_OUTER_BOUND('',#6928,.T.);
#5758=FACE_OUTER_BOUND('',#6929,.T.);
#5759=FACE_OUTER_BOUND('',#6931,.T.);
#5760=FACE_OUTER_BOUND('',#6932,.T.);
#5761=FACE_OUTER_BOUND('',#6933,.T.);
#5762=FACE_OUTER_BOUND('',#6934,.T.);
#5763=FACE_OUTER_BOUND('',#6935,.T.);
#5764=FACE_OUTER_BOUND('',#6936,.T.);
#5765=FACE_OUTER_BOUND('',#6937,.T.);
#5766=FACE_OUTER_BOUND('',#6939,.T.);
#5767=FACE_OUTER_BOUND('',#6940,.T.);
#5768=FACE_OUTER_BOUND('',#6941,.T.);
#5769=FACE_OUTER_BOUND('',#6942,.T.);
#5770=FACE_OUTER_BOUND('',#6944,.T.);
#5771=FACE_OUTER_BOUND('',#6945,.T.);
#5772=FACE_OUTER_BOUND('',#6946,.T.);
#5773=FACE_OUTER_BOUND('',#6947,.T.);
#5774=FACE_OUTER_BOUND('',#6948,.T.);
#5775=FACE_OUTER_BOUND('',#6950,.T.);
#5776=FACE_OUTER_BOUND('',#6951,.T.);
#5777=FACE_OUTER_BOUND('',#6952,.T.);
#5778=FACE_OUTER_BOUND('',#6955,.T.);
#5779=FACE_OUTER_BOUND('',#6956,.T.);
#5780=FACE_OUTER_BOUND('',#6957,.T.);
#5781=FACE_OUTER_BOUND('',#6958,.T.);
#5782=FACE_OUTER_BOUND('',#6959,.T.);
#5783=FACE_OUTER_BOUND('',#6960,.T.);
#5784=FACE_OUTER_BOUND('',#6961,.T.);
#5785=FACE_OUTER_BOUND('',#6962,.T.);
#5786=FACE_OUTER_BOUND('',#6963,.T.);
#5787=FACE_OUTER_BOUND('',#6964,.T.);
#5788=FACE_OUTER_BOUND('',#6965,.T.);
#5789=FACE_OUTER_BOUND('',#6966,.T.);
#5790=FACE_OUTER_BOUND('',#6971,.T.);
#5791=FACE_OUTER_BOUND('',#6972,.T.);
#5792=FACE_OUTER_BOUND('',#6973,.T.);
#5793=FACE_OUTER_BOUND('',#6974,.T.);
#5794=FACE_OUTER_BOUND('',#6975,.T.);
#5795=FACE_OUTER_BOUND('',#6977,.T.);
#5796=FACE_OUTER_BOUND('',#6978,.T.);
#5797=FACE_OUTER_BOUND('',#6979,.T.);
#5798=FACE_OUTER_BOUND('',#6980,.T.);
#5799=FACE_OUTER_BOUND('',#6981,.T.);
#5800=FACE_OUTER_BOUND('',#6982,.T.);
#5801=FACE_OUTER_BOUND('',#6983,.T.);
#5802=FACE_OUTER_BOUND('',#6984,.T.);
#5803=FACE_OUTER_BOUND('',#6985,.T.);
#5804=FACE_OUTER_BOUND('',#6986,.T.);
#5805=FACE_OUTER_BOUND('',#6987,.T.);
#5806=FACE_OUTER_BOUND('',#6988,.T.);
#5807=FACE_OUTER_BOUND('',#6989,.T.);
#5808=FACE_OUTER_BOUND('',#6990,.T.);
#5809=FACE_OUTER_BOUND('',#6991,.T.);
#5810=FACE_OUTER_BOUND('',#6992,.T.);
#5811=FACE_OUTER_BOUND('',#6993,.T.);
#5812=FACE_OUTER_BOUND('',#6994,.T.);
#5813=FACE_OUTER_BOUND('',#6995,.T.);
#5814=FACE_OUTER_BOUND('',#6996,.T.);
#5815=EDGE_LOOP('',(#12006,#12007,#12008,#12009));
#5816=EDGE_LOOP('',(#12010,#12011,#12012,#12013,#12014));
#5817=EDGE_LOOP('',(#12015,#12016,#12017,#12018,#12019,#12020,#12021,#12022,
#12023,#12024,#12025,#12026,#12027,#12028,#12029,#12030,#12031,#12032,#12033,
#12034,#12035,#12036,#12037,#12038,#12039,#12040,#12041,#12042,#12043,#12044,
#12045,#12046,#12047,#12048,#12049,#12050,#12051,#12052,#12053,#12054));
#5818=EDGE_LOOP('',(#12055,#12056,#12057,#12058));
#5819=EDGE_LOOP('',(#12059,#12060,#12061,#12062));
#5820=EDGE_LOOP('',(#12063,#12064,#12065,#12066));
#5821=EDGE_LOOP('',(#12067,#12068,#12069,#12070));
#5822=EDGE_LOOP('',(#12071,#12072,#12073,#12074));
#5823=EDGE_LOOP('',(#12075,#12076,#12077,#12078));
#5824=EDGE_LOOP('',(#12079,#12080,#12081,#12082));
#5825=EDGE_LOOP('',(#12083,#12084,#12085,#12086));
#5826=EDGE_LOOP('',(#12087,#12088,#12089,#12090));
#5827=EDGE_LOOP('',(#12091,#12092,#12093,#12094));
#5828=EDGE_LOOP('',(#12095,#12096,#12097,#12098));
#5829=EDGE_LOOP('',(#12099,#12100,#12101,#12102));
#5830=EDGE_LOOP('',(#12103,#12104,#12105,#12106));
#5831=EDGE_LOOP('',(#12107,#12108,#12109,#12110));
#5832=EDGE_LOOP('',(#12111,#12112,#12113,#12114));
#5833=EDGE_LOOP('',(#12115,#12116,#12117,#12118));
#5834=EDGE_LOOP('',(#12119,#12120,#12121,#12122));
#5835=EDGE_LOOP('',(#12123,#12124,#12125,#12126));
#5836=EDGE_LOOP('',(#12127,#12128,#12129,#12130));
#5837=EDGE_LOOP('',(#12131,#12132,#12133,#12134));
#5838=EDGE_LOOP('',(#12135,#12136,#12137,#12138));
#5839=EDGE_LOOP('',(#12139,#12140,#12141,#12142));
#5840=EDGE_LOOP('',(#12143,#12144,#12145,#12146));
#5841=EDGE_LOOP('',(#12147,#12148,#12149,#12150));
#5842=EDGE_LOOP('',(#12151,#12152,#12153,#12154));
#5843=EDGE_LOOP('',(#12155,#12156,#12157,#12158));
#5844=EDGE_LOOP('',(#12159,#12160,#12161,#12162));
#5845=EDGE_LOOP('',(#12163,#12164,#12165,#12166));
#5846=EDGE_LOOP('',(#12167,#12168,#12169,#12170,#12171));
#5847=EDGE_LOOP('',(#12172));
#5848=EDGE_LOOP('',(#12173));
#5849=EDGE_LOOP('',(#12174,#12175,#12176,#12177));
#5850=EDGE_LOOP('',(#12178,#12179,#12180,#12181));
#5851=EDGE_LOOP('',(#12182));
#5852=EDGE_LOOP('',(#12183));
#5853=EDGE_LOOP('',(#12184));
#5854=EDGE_LOOP('',(#12185,#12186,#12187,#12188,#12189,#12190,#12191,#12192,
#12193,#12194,#12195,#12196,#12197,#12198,#12199,#12200,#12201,#12202,#12203,
#12204,#12205,#12206,#12207,#12208,#12209,#12210,#12211,#12212,#12213,#12214,
#12215,#12216,#12217,#12218,#12219,#12220,#12221));
#5855=EDGE_LOOP('',(#12222));
#5856=EDGE_LOOP('',(#12223));
#5857=EDGE_LOOP('',(#12224));
#5858=EDGE_LOOP('',(#12225));
#5859=EDGE_LOOP('',(#12226));
#5860=EDGE_LOOP('',(#12227));
#5861=EDGE_LOOP('',(#12228));
#5862=EDGE_LOOP('',(#12229));
#5863=EDGE_LOOP('',(#12230));
#5864=EDGE_LOOP('',(#12231));
#5865=EDGE_LOOP('',(#12232));
#5866=EDGE_LOOP('',(#12233));
#5867=EDGE_LOOP('',(#12234));
#5868=EDGE_LOOP('',(#12235));
#5869=EDGE_LOOP('',(#12236));
#5870=EDGE_LOOP('',(#12237));
#5871=EDGE_LOOP('',(#12238));
#5872=EDGE_LOOP('',(#12239));
#5873=EDGE_LOOP('',(#12240));
#5874=EDGE_LOOP('',(#12241));
#5875=EDGE_LOOP('',(#12242));
#5876=EDGE_LOOP('',(#12243));
#5877=EDGE_LOOP('',(#12244));
#5878=EDGE_LOOP('',(#12245));
#5879=EDGE_LOOP('',(#12246));
#5880=EDGE_LOOP('',(#12247));
#5881=EDGE_LOOP('',(#12248));
#5882=EDGE_LOOP('',(#12249));
#5883=EDGE_LOOP('',(#12250));
#5884=EDGE_LOOP('',(#12251));
#5885=EDGE_LOOP('',(#12252));
#5886=EDGE_LOOP('',(#12253));
#5887=EDGE_LOOP('',(#12254));
#5888=EDGE_LOOP('',(#12255));
#5889=EDGE_LOOP('',(#12256));
#5890=EDGE_LOOP('',(#12257));
#5891=EDGE_LOOP('',(#12258,#12259,#12260,#12261,#12262,#12263,#12264,#12265));
#5892=EDGE_LOOP('',(#12266));
#5893=EDGE_LOOP('',(#12267));
#5894=EDGE_LOOP('',(#12268));
#5895=EDGE_LOOP('',(#12269));
#5896=EDGE_LOOP('',(#12270));
#5897=EDGE_LOOP('',(#12271,#12272,#12273,#12274,#12275,#12276,#12277,#12278));
#5898=EDGE_LOOP('',(#12279));
#5899=EDGE_LOOP('',(#12280));
#5900=EDGE_LOOP('',(#12281));
#5901=EDGE_LOOP('',(#12282));
#5902=EDGE_LOOP('',(#12283));
#5903=EDGE_LOOP('',(#12284,#12285,#12286,#12287));
#5904=EDGE_LOOP('',(#12288,#12289,#12290,#12291));
#5905=EDGE_LOOP('',(#12292,#12293,#12294,#12295));
#5906=EDGE_LOOP('',(#12296,#12297,#12298,#12299));
#5907=EDGE_LOOP('',(#12300,#12301,#12302,#12303));
#5908=EDGE_LOOP('',(#12304,#12305,#12306,#12307));
#5909=EDGE_LOOP('',(#12308,#12309,#12310,#12311));
#5910=EDGE_LOOP('',(#12312,#12313,#12314,#12315));
#5911=EDGE_LOOP('',(#12316,#12317,#12318,#12319,#12320,#12321,#12322,#12323));
#5912=EDGE_LOOP('',(#12324));
#5913=EDGE_LOOP('',(#12325));
#5914=EDGE_LOOP('',(#12326));
#5915=EDGE_LOOP('',(#12327));
#5916=EDGE_LOOP('',(#12328));
#5917=EDGE_LOOP('',(#12329,#12330,#12331,#12332,#12333,#12334,#12335,#12336));
#5918=EDGE_LOOP('',(#12337));
#5919=EDGE_LOOP('',(#12338));
#5920=EDGE_LOOP('',(#12339));
#5921=EDGE_LOOP('',(#12340));
#5922=EDGE_LOOP('',(#12341));
#5923=EDGE_LOOP('',(#12342,#12343,#12344,#12345));
#5924=EDGE_LOOP('',(#12346,#12347,#12348,#12349));
#5925=EDGE_LOOP('',(#12350,#12351,#12352,#12353));
#5926=EDGE_LOOP('',(#12354,#12355,#12356,#12357));
#5927=EDGE_LOOP('',(#12358,#12359,#12360,#12361));
#5928=EDGE_LOOP('',(#12362,#12363,#12364,#12365));
#5929=EDGE_LOOP('',(#12366,#12367,#12368,#12369));
#5930=EDGE_LOOP('',(#12370,#12371,#12372,#12373));
#5931=EDGE_LOOP('',(#12374));
#5932=EDGE_LOOP('',(#12375));
#5933=EDGE_LOOP('',(#12376,#12377,#12378));
#5934=EDGE_LOOP('',(#12379,#12380,#12381));
#5935=EDGE_LOOP('',(#12382,#12383,#12384,#12385));
#5936=EDGE_LOOP('',(#12386,#12387,#12388));
#5937=EDGE_LOOP('',(#12389,#12390,#12391));
#5938=EDGE_LOOP('',(#12392,#12393,#12394,#12395));
#5939=EDGE_LOOP('',(#12396,#12397,#12398));
#5940=EDGE_LOOP('',(#12399,#12400,#12401));
#5941=EDGE_LOOP('',(#12402,#12403,#12404,#12405));
#5942=EDGE_LOOP('',(#12406,#12407,#12408));
#5943=EDGE_LOOP('',(#12409,#12410,#12411));
#5944=EDGE_LOOP('',(#12412,#12413,#12414,#12415));
#5945=EDGE_LOOP('',(#12416,#12417,#12418));
#5946=EDGE_LOOP('',(#12419,#12420,#12421));
#5947=EDGE_LOOP('',(#12422,#12423,#12424,#12425));
#5948=EDGE_LOOP('',(#12426,#12427,#12428));
#5949=EDGE_LOOP('',(#12429,#12430,#12431));
#5950=EDGE_LOOP('',(#12432,#12433,#12434,#12435));
#5951=EDGE_LOOP('',(#12436,#12437,#12438));
#5952=EDGE_LOOP('',(#12439,#12440,#12441));
#5953=EDGE_LOOP('',(#12442,#12443,#12444,#12445));
#5954=EDGE_LOOP('',(#12446,#12447,#12448));
#5955=EDGE_LOOP('',(#12449,#12450,#12451));
#5956=EDGE_LOOP('',(#12452,#12453,#12454,#12455));
#5957=EDGE_LOOP('',(#12456,#12457,#12458));
#5958=EDGE_LOOP('',(#12459,#12460,#12461));
#5959=EDGE_LOOP('',(#12462,#12463,#12464,#12465));
#5960=EDGE_LOOP('',(#12466,#12467,#12468,#12469));
#5961=EDGE_LOOP('',(#12470,#12471,#12472,#12473));
#5962=EDGE_LOOP('',(#12474,#12475,#12476,#12477,#12478,#12479,#12480,#12481,
#12482,#12483,#12484));
#5963=EDGE_LOOP('',(#12485,#12486,#12487,#12488));
#5964=EDGE_LOOP('',(#12489,#12490));
#5965=EDGE_LOOP('',(#12491,#12492));
#5966=EDGE_LOOP('',(#12493,#12494));
#5967=EDGE_LOOP('',(#12495,#12496));
#5968=EDGE_LOOP('',(#12497));
#5969=EDGE_LOOP('',(#12498,#12499,#12500,#12501));
#5970=EDGE_LOOP('',(#12502,#12503,#12504,#12505));
#5971=EDGE_LOOP('',(#12506,#12507));
#5972=EDGE_LOOP('',(#12508,#12509));
#5973=EDGE_LOOP('',(#12510,#12511));
#5974=EDGE_LOOP('',(#12512,#12513));
#5975=EDGE_LOOP('',(#12514,#12515));
#5976=EDGE_LOOP('',(#12516,#12517));
#5977=EDGE_LOOP('',(#12518,#12519));
#5978=EDGE_LOOP('',(#12520,#12521));
#5979=EDGE_LOOP('',(#12522,#12523));
#5980=EDGE_LOOP('',(#12524,#12525));
#5981=EDGE_LOOP('',(#12526,#12527,#12528,#12529));
#5982=EDGE_LOOP('',(#12530,#12531,#12532,#12533));
#5983=EDGE_LOOP('',(#12534,#12535,#12536,#12537,#12538,#12539,#12540,#12541,
#12542,#12543,#12544));
#5984=EDGE_LOOP('',(#12545,#12546,#12547,#12548));
#5985=EDGE_LOOP('',(#12549,#12550,#12551));
#5986=EDGE_LOOP('',(#12552,#12553));
#5987=EDGE_LOOP('',(#12554,#12555,#12556));
#5988=EDGE_LOOP('',(#12557,#12558));
#5989=EDGE_LOOP('',(#12559));
#5990=EDGE_LOOP('',(#12560,#12561,#12562,#12563));
#5991=EDGE_LOOP('',(#12564,#12565,#12566,#12567));
#5992=EDGE_LOOP('',(#12568,#12569));
#5993=EDGE_LOOP('',(#12570,#12571));
#5994=EDGE_LOOP('',(#12572,#12573));
#5995=EDGE_LOOP('',(#12574,#12575));
#5996=EDGE_LOOP('',(#12576,#12577));
#5997=EDGE_LOOP('',(#12578,#12579));
#5998=EDGE_LOOP('',(#12580,#12581));
#5999=EDGE_LOOP('',(#12582,#12583));
#6000=EDGE_LOOP('',(#12584,#12585));
#6001=EDGE_LOOP('',(#12586,#12587));
#6002=EDGE_LOOP('',(#12588,#12589,#12590,#12591,#12592,#12593,#12594));
#6003=EDGE_LOOP('',(#12595,#12596,#12597,#12598));
#6004=EDGE_LOOP('',(#12599,#12600,#12601,#12602));
#6005=EDGE_LOOP('',(#12603,#12604,#12605,#12606,#12607,#12608,#12609));
#6006=EDGE_LOOP('',(#12610,#12611,#12612,#12613));
#6007=EDGE_LOOP('',(#12614,#12615,#12616,#12617));
#6008=EDGE_LOOP('',(#12618,#12619,#12620,#12621));
#6009=EDGE_LOOP('',(#12622,#12623,#12624,#12625,#12626,#12627,#12628,#12629,
#12630,#12631,#12632,#12633));
#6010=EDGE_LOOP('',(#12634,#12635,#12636,#12637));
#6011=EDGE_LOOP('',(#12638,#12639,#12640,#12641,#12642,#12643,#12644,#12645,
#12646));
#6012=EDGE_LOOP('',(#12647,#12648));
#6013=EDGE_LOOP('',(#12649,#12650,#12651,#12652));
#6014=EDGE_LOOP('',(#12653,#12654,#12655,#12656));
#6015=EDGE_LOOP('',(#12657,#12658,#12659,#12660));
#6016=EDGE_LOOP('',(#12661,#12662,#12663,#12664));
#6017=EDGE_LOOP('',(#12665,#12666,#12667,#12668,#12669,#12670,#12671,#12672,
#12673,#12674,#12675,#12676,#12677,#12678,#12679,#12680));
#6018=EDGE_LOOP('',(#12681,#12682,#12683,#12684,#12685,#12686,#12687,#12688,
#12689,#12690,#12691,#12692,#12693,#12694,#12695,#12696,#12697,#12698,#12699,
#12700,#12701,#12702,#12703,#12704,#12705,#12706,#12707,#12708,#12709,#12710,
#12711,#12712,#12713,#12714,#12715,#12716,#12717,#12718,#12719));
#6019=EDGE_LOOP('',(#12720,#12721,#12722,#12723));
#6020=EDGE_LOOP('',(#12724,#12725,#12726,#12727));
#6021=EDGE_LOOP('',(#12728,#12729,#12730,#12731));
#6022=EDGE_LOOP('',(#12732,#12733,#12734,#12735));
#6023=EDGE_LOOP('',(#12736,#12737,#12738,#12739));
#6024=EDGE_LOOP('',(#12740,#12741,#12742,#12743));
#6025=EDGE_LOOP('',(#12744,#12745,#12746,#12747));
#6026=EDGE_LOOP('',(#12748,#12749,#12750,#12751));
#6027=EDGE_LOOP('',(#12752));
#6028=EDGE_LOOP('',(#12753));
#6029=EDGE_LOOP('',(#12754));
#6030=EDGE_LOOP('',(#12755));
#6031=EDGE_LOOP('',(#12756,#12757,#12758,#12759));
#6032=EDGE_LOOP('',(#12760,#12761,#12762,#12763));
#6033=EDGE_LOOP('',(#12764,#12765,#12766,#12767));
#6034=EDGE_LOOP('',(#12768,#12769,#12770,#12771));
#6035=EDGE_LOOP('',(#12772,#12773,#12774,#12775));
#6036=EDGE_LOOP('',(#12776,#12777,#12778,#12779));
#6037=EDGE_LOOP('',(#12780,#12781,#12782,#12783,#12784,#12785,#12786,#12787,
#12788,#12789,#12790,#12791,#12792,#12793,#12794,#12795));
#6038=EDGE_LOOP('',(#12796,#12797,#12798,#12799));
#6039=EDGE_LOOP('',(#12800,#12801,#12802,#12803,#12804,#12805,#12806,#12807,
#12808,#12809,#12810,#12811,#12812,#12813,#12814,#12815,#12816,#12817,#12818,
#12819,#12820,#12821,#12822,#12823,#12824,#12825,#12826,#12827,#12828,#12829,
#12830,#12831,#12832,#12833,#12834,#12835,#12836,#12837,#12838));
#6040=EDGE_LOOP('',(#12839,#12840,#12841,#12842));
#6041=EDGE_LOOP('',(#12843,#12844,#12845,#12846));
#6042=EDGE_LOOP('',(#12847,#12848,#12849,#12850));
#6043=EDGE_LOOP('',(#12851,#12852,#12853,#12854));
#6044=EDGE_LOOP('',(#12855,#12856,#12857,#12858));
#6045=EDGE_LOOP('',(#12859,#12860,#12861,#12862));
#6046=EDGE_LOOP('',(#12863,#12864,#12865,#12866));
#6047=EDGE_LOOP('',(#12867,#12868,#12869,#12870));
#6048=EDGE_LOOP('',(#12871,#12872,#12873,#12874));
#6049=EDGE_LOOP('',(#12875,#12876,#12877,#12878));
#6050=EDGE_LOOP('',(#12879,#12880,#12881,#12882));
#6051=EDGE_LOOP('',(#12883,#12884,#12885,#12886));
#6052=EDGE_LOOP('',(#12887,#12888,#12889,#12890));
#6053=EDGE_LOOP('',(#12891,#12892,#12893,#12894));
#6054=EDGE_LOOP('',(#12895,#12896,#12897,#12898));
#6055=EDGE_LOOP('',(#12899,#12900,#12901,#12902));
#6056=EDGE_LOOP('',(#12903,#12904,#12905,#12906));
#6057=EDGE_LOOP('',(#12907,#12908,#12909,#12910));
#6058=EDGE_LOOP('',(#12911,#12912,#12913,#12914));
#6059=EDGE_LOOP('',(#12915,#12916,#12917,#12918));
#6060=EDGE_LOOP('',(#12919,#12920,#12921,#12922));
#6061=EDGE_LOOP('',(#12923,#12924,#12925,#12926));
#6062=EDGE_LOOP('',(#12927,#12928,#12929,#12930));
#6063=EDGE_LOOP('',(#12931,#12932,#12933,#12934));
#6064=EDGE_LOOP('',(#12935,#12936,#12937,#12938));
#6065=EDGE_LOOP('',(#12939,#12940,#12941,#12942));
#6066=EDGE_LOOP('',(#12943,#12944,#12945,#12946));
#6067=EDGE_LOOP('',(#12947,#12948,#12949,#12950));
#6068=EDGE_LOOP('',(#12951,#12952,#12953,#12954));
#6069=EDGE_LOOP('',(#12955,#12956,#12957,#12958));
#6070=EDGE_LOOP('',(#12959,#12960,#12961,#12962));
#6071=EDGE_LOOP('',(#12963,#12964,#12965,#12966));
#6072=EDGE_LOOP('',(#12967,#12968,#12969,#12970,#12971,#12972,#12973,#12974));
#6073=EDGE_LOOP('',(#12975,#12976,#12977,#12978));
#6074=EDGE_LOOP('',(#12979,#12980,#12981,#12982));
#6075=EDGE_LOOP('',(#12983,#12984,#12985,#12986,#12987,#12988,#12989));
#6076=EDGE_LOOP('',(#12990,#12991,#12992,#12993));
#6077=EDGE_LOOP('',(#12994,#12995,#12996,#12997));
#6078=EDGE_LOOP('',(#12998,#12999,#13000,#13001));
#6079=EDGE_LOOP('',(#13002,#13003,#13004,#13005,#13006,#13007,#13008,#13009,
#13010,#13011,#13012,#13013));
#6080=EDGE_LOOP('',(#13014,#13015,#13016,#13017,#13018,#13019,#13020,#13021,
#13022,#13023,#13024,#13025));
#6081=EDGE_LOOP('',(#13026,#13027,#13028,#13029,#13030));
#6082=EDGE_LOOP('',(#13031,#13032,#13033,#13034,#13035));
#6083=EDGE_LOOP('',(#13036,#13037,#13038,#13039,#13040));
#6084=EDGE_LOOP('',(#13041,#13042,#13043,#13044,#13045));
#6085=EDGE_LOOP('',(#13046,#13047,#13048,#13049,#13050));
#6086=EDGE_LOOP('',(#13051,#13052,#13053,#13054,#13055));
#6087=EDGE_LOOP('',(#13056));
#6088=EDGE_LOOP('',(#13057));
#6089=EDGE_LOOP('',(#13058));
#6090=EDGE_LOOP('',(#13059));
#6091=EDGE_LOOP('',(#13060,#13061));
#6092=EDGE_LOOP('',(#13062,#13063,#13064,#13065,#13066));
#6093=EDGE_LOOP('',(#13067,#13068));
#6094=EDGE_LOOP('',(#13069,#13070,#13071,#13072,#13073));
#6095=EDGE_LOOP('',(#13074,#13075,#13076,#13077));
#6096=EDGE_LOOP('',(#13078,#13079,#13080,#13081));
#6097=EDGE_LOOP('',(#13082,#13083,#13084,#13085));
#6098=EDGE_LOOP('',(#13086,#13087,#13088,#13089));
#6099=EDGE_LOOP('',(#13090,#13091,#13092,#13093,#13094,#13095,#13096,#13097,
#13098,#13099,#13100,#13101));
#6100=EDGE_LOOP('',(#13102,#13103,#13104,#13105,#13106,#13107,#13108,#13109,
#13110,#13111,#13112,#13113));
#6101=EDGE_LOOP('',(#13114,#13115,#13116,#13117));
#6102=EDGE_LOOP('',(#13118,#13119,#13120,#13121));
#6103=EDGE_LOOP('',(#13122,#13123,#13124,#13125));
#6104=EDGE_LOOP('',(#13126,#13127,#13128,#13129));
#6105=EDGE_LOOP('',(#13130,#13131,#13132,#13133));
#6106=EDGE_LOOP('',(#13134,#13135,#13136,#13137));
#6107=EDGE_LOOP('',(#13138,#13139,#13140,#13141));
#6108=EDGE_LOOP('',(#13142,#13143,#13144,#13145));
#6109=EDGE_LOOP('',(#13146,#13147,#13148,#13149));
#6110=EDGE_LOOP('',(#13150,#13151,#13152,#13153));
#6111=EDGE_LOOP('',(#13154,#13155,#13156,#13157,#13158,#13159,#13160,#13161,
#13162,#13163,#13164,#13165));
#6112=EDGE_LOOP('',(#13166));
#6113=EDGE_LOOP('',(#13167));
#6114=EDGE_LOOP('',(#13168));
#6115=EDGE_LOOP('',(#13169));
#6116=EDGE_LOOP('',(#13170,#13171,#13172,#13173,#13174,#13175,#13176,#13177,
#13178,#13179,#13180,#13181,#13182,#13183,#13184,#13185,#13186,#13187));
#6117=EDGE_LOOP('',(#13188));
#6118=EDGE_LOOP('',(#13189));
#6119=EDGE_LOOP('',(#13190));
#6120=EDGE_LOOP('',(#13191));
#6121=EDGE_LOOP('',(#13192,#13193,#13194,#13195));
#6122=EDGE_LOOP('',(#13196,#13197,#13198,#13199));
#6123=EDGE_LOOP('',(#13200,#13201,#13202,#13203,#13204,#13205,#13206,#13207));
#6124=EDGE_LOOP('',(#13208,#13209,#13210,#13211,#13212,#13213,#13214,#13215));
#6125=EDGE_LOOP('',(#13216,#13217,#13218,#13219));
#6126=EDGE_LOOP('',(#13220,#13221,#13222,#13223));
#6127=EDGE_LOOP('',(#13224,#13225,#13226,#13227,#13228,#13229,#13230));
#6128=EDGE_LOOP('',(#13231,#13232,#13233,#13234));
#6129=EDGE_LOOP('',(#13235,#13236,#13237,#13238));
#6130=EDGE_LOOP('',(#13239,#13240,#13241,#13242));
#6131=EDGE_LOOP('',(#13243,#13244,#13245,#13246));
#6132=EDGE_LOOP('',(#13247,#13248,#13249,#13250,#13251,#13252,#13253));
#6133=EDGE_LOOP('',(#13254,#13255,#13256,#13257));
#6134=EDGE_LOOP('',(#13258,#13259,#13260,#13261));
#6135=EDGE_LOOP('',(#13262,#13263,#13264,#13265));
#6136=EDGE_LOOP('',(#13266,#13267,#13268,#13269));
#6137=EDGE_LOOP('',(#13270,#13271,#13272,#13273));
#6138=EDGE_LOOP('',(#13274,#13275,#13276,#13277));
#6139=EDGE_LOOP('',(#13278,#13279,#13280,#13281));
#6140=EDGE_LOOP('',(#13282,#13283,#13284,#13285));
#6141=EDGE_LOOP('',(#13286,#13287,#13288,#13289));
#6142=EDGE_LOOP('',(#13290,#13291,#13292,#13293));
#6143=EDGE_LOOP('',(#13294,#13295,#13296,#13297));
#6144=EDGE_LOOP('',(#13298,#13299,#13300,#13301));
#6145=EDGE_LOOP('',(#13302,#13303,#13304,#13305));
#6146=EDGE_LOOP('',(#13306,#13307,#13308,#13309));
#6147=EDGE_LOOP('',(#13310,#13311,#13312,#13313));
#6148=EDGE_LOOP('',(#13314,#13315,#13316,#13317));
#6149=EDGE_LOOP('',(#13318,#13319,#13320,#13321));
#6150=EDGE_LOOP('',(#13322,#13323,#13324,#13325));
#6151=EDGE_LOOP('',(#13326,#13327,#13328,#13329));
#6152=EDGE_LOOP('',(#13330));
#6153=EDGE_LOOP('',(#13331));
#6154=EDGE_LOOP('',(#13332));
#6155=EDGE_LOOP('',(#13333));
#6156=EDGE_LOOP('',(#13334));
#6157=EDGE_LOOP('',(#13335));
#6158=EDGE_LOOP('',(#13336));
#6159=EDGE_LOOP('',(#13337));
#6160=EDGE_LOOP('',(#13338));
#6161=EDGE_LOOP('',(#13339));
#6162=EDGE_LOOP('',(#13340));
#6163=EDGE_LOOP('',(#13341));
#6164=EDGE_LOOP('',(#13342));
#6165=EDGE_LOOP('',(#13343));
#6166=EDGE_LOOP('',(#13344));
#6167=EDGE_LOOP('',(#13345));
#6168=EDGE_LOOP('',(#13346));
#6169=EDGE_LOOP('',(#13347));
#6170=EDGE_LOOP('',(#13348));
#6171=EDGE_LOOP('',(#13349));
#6172=EDGE_LOOP('',(#13350));
#6173=EDGE_LOOP('',(#13351));
#6174=EDGE_LOOP('',(#13352));
#6175=EDGE_LOOP('',(#13353));
#6176=EDGE_LOOP('',(#13354));
#6177=EDGE_LOOP('',(#13355));
#6178=EDGE_LOOP('',(#13356));
#6179=EDGE_LOOP('',(#13357));
#6180=EDGE_LOOP('',(#13358));
#6181=EDGE_LOOP('',(#13359));
#6182=EDGE_LOOP('',(#13360));
#6183=EDGE_LOOP('',(#13361));
#6184=EDGE_LOOP('',(#13362));
#6185=EDGE_LOOP('',(#13363));
#6186=EDGE_LOOP('',(#13364,#13365,#13366,#13367));
#6187=EDGE_LOOP('',(#13368));
#6188=EDGE_LOOP('',(#13369));
#6189=EDGE_LOOP('',(#13370,#13371,#13372,#13373,#13374));
#6190=EDGE_LOOP('',(#13375,#13376,#13377,#13378,#13379,#13380));
#6191=EDGE_LOOP('',(#13381,#13382,#13383,#13384,#13385,#13386));
#6192=EDGE_LOOP('',(#13387,#13388,#13389,#13390,#13391,#13392));
#6193=EDGE_LOOP('',(#13393,#13394,#13395,#13396));
#6194=EDGE_LOOP('',(#13397,#13398,#13399,#13400,#13401,#13402));
#6195=EDGE_LOOP('',(#13403,#13404,#13405,#13406,#13407));
#6196=EDGE_LOOP('',(#13408,#13409,#13410,#13411,#13412,#13413));
#6197=EDGE_LOOP('',(#13414,#13415,#13416,#13417,#13418,#13419));
#6198=EDGE_LOOP('',(#13420));
#6199=EDGE_LOOP('',(#13421));
#6200=EDGE_LOOP('',(#13422));
#6201=EDGE_LOOP('',(#13423));
#6202=EDGE_LOOP('',(#13424,#13425,#13426,#13427,#13428));
#6203=EDGE_LOOP('',(#13429,#13430,#13431,#13432,#13433));
#6204=EDGE_LOOP('',(#13434));
#6205=EDGE_LOOP('',(#13435));
#6206=EDGE_LOOP('',(#13436,#13437,#13438));
#6207=EDGE_LOOP('',(#13439));
#6208=EDGE_LOOP('',(#13440,#13441,#13442,#13443,#13444,#13445));
#6209=EDGE_LOOP('',(#13446,#13447,#13448,#13449));
#6210=EDGE_LOOP('',(#13450,#13451,#13452,#13453));
#6211=EDGE_LOOP('',(#13454,#13455,#13456,#13457,#13458));
#6212=EDGE_LOOP('',(#13459,#13460,#13461,#13462));
#6213=EDGE_LOOP('',(#13463,#13464,#13465,#13466));
#6214=EDGE_LOOP('',(#13467,#13468,#13469,#13470,#13471));
#6215=EDGE_LOOP('',(#13472,#13473,#13474,#13475,#13476));
#6216=EDGE_LOOP('',(#13477,#13478,#13479,#13480,#13481));
#6217=EDGE_LOOP('',(#13482,#13483,#13484,#13485,#13486));
#6218=EDGE_LOOP('',(#13487,#13488,#13489,#13490,#13491,#13492));
#6219=EDGE_LOOP('',(#13493,#13494,#13495,#13496,#13497));
#6220=EDGE_LOOP('',(#13498,#13499,#13500,#13501));
#6221=EDGE_LOOP('',(#13502,#13503,#13504,#13505));
#6222=EDGE_LOOP('',(#13506,#13507,#13508,#13509));
#6223=EDGE_LOOP('',(#13510,#13511,#13512,#13513));
#6224=EDGE_LOOP('',(#13514,#13515,#13516,#13517,#13518,#13519));
#6225=EDGE_LOOP('',(#13520,#13521,#13522,#13523));
#6226=EDGE_LOOP('',(#13524,#13525,#13526,#13527,#13528,#13529,#13530,#13531));
#6227=EDGE_LOOP('',(#13532,#13533,#13534,#13535));
#6228=EDGE_LOOP('',(#13536,#13537,#13538,#13539));
#6229=EDGE_LOOP('',(#13540,#13541,#13542,#13543,#13544,#13545,#13546,#13547,
#13548,#13549));
#6230=EDGE_LOOP('',(#13550,#13551,#13552,#13553,#13554,#13555,#13556,#13557));
#6231=EDGE_LOOP('',(#13558,#13559,#13560,#13561));
#6232=EDGE_LOOP('',(#13562,#13563,#13564,#13565));
#6233=EDGE_LOOP('',(#13566,#13567,#13568,#13569));
#6234=EDGE_LOOP('',(#13570,#13571,#13572,#13573));
#6235=EDGE_LOOP('',(#13574,#13575,#13576,#13577,#13578,#13579,#13580,#13581));
#6236=EDGE_LOOP('',(#13582,#13583,#13584,#13585));
#6237=EDGE_LOOP('',(#13586,#13587,#13588,#13589));
#6238=EDGE_LOOP('',(#13590,#13591,#13592,#13593,#13594));
#6239=EDGE_LOOP('',(#13595,#13596,#13597,#13598));
#6240=EDGE_LOOP('',(#13599,#13600,#13601,#13602));
#6241=EDGE_LOOP('',(#13603,#13604,#13605,#13606));
#6242=EDGE_LOOP('',(#13607,#13608,#13609,#13610));
#6243=EDGE_LOOP('',(#13611,#13612,#13613,#13614));
#6244=EDGE_LOOP('',(#13615,#13616,#13617,#13618));
#6245=EDGE_LOOP('',(#13619,#13620,#13621,#13622,#13623,#13624));
#6246=EDGE_LOOP('',(#13625,#13626,#13627,#13628,#13629,#13630));
#6247=EDGE_LOOP('',(#13631,#13632,#13633,#13634,#13635,#13636,#13637,#13638,
#13639,#13640,#13641,#13642,#13643,#13644,#13645,#13646,#13647,#13648,#13649,
#13650,#13651,#13652,#13653,#13654));
#6248=EDGE_LOOP('',(#13655,#13656));
#6249=EDGE_LOOP('',(#13657,#13658,#13659,#13660,#13661,#13662,#13663,#13664));
#6250=EDGE_LOOP('',(#13665,#13666,#13667,#13668));
#6251=EDGE_LOOP('',(#13669,#13670,#13671,#13672,#13673,#13674,#13675,#13676));
#6252=EDGE_LOOP('',(#13677,#13678,#13679,#13680,#13681,#13682));
#6253=EDGE_LOOP('',(#13683,#13684,#13685,#13686));
#6254=EDGE_LOOP('',(#13687,#13688,#13689,#13690));
#6255=EDGE_LOOP('',(#13691,#13692,#13693,#13694));
#6256=EDGE_LOOP('',(#13695,#13696,#13697,#13698));
#6257=EDGE_LOOP('',(#13699,#13700,#13701,#13702,#13703,#13704,#13705,#13706,
#13707,#13708,#13709,#13710));
#6258=EDGE_LOOP('',(#13711,#13712,#13713,#13714));
#6259=EDGE_LOOP('',(#13715,#13716,#13717,#13718));
#6260=EDGE_LOOP('',(#13719,#13720,#13721,#13722));
#6261=EDGE_LOOP('',(#13723,#13724,#13725,#13726));
#6262=EDGE_LOOP('',(#13727,#13728,#13729,#13730));
#6263=EDGE_LOOP('',(#13731,#13732,#13733,#13734));
#6264=EDGE_LOOP('',(#13735,#13736,#13737,#13738));
#6265=EDGE_LOOP('',(#13739,#13740,#13741,#13742));
#6266=EDGE_LOOP('',(#13743,#13744,#13745,#13746));
#6267=EDGE_LOOP('',(#13747,#13748,#13749,#13750));
#6268=EDGE_LOOP('',(#13751,#13752,#13753,#13754,#13755,#13756));
#6269=EDGE_LOOP('',(#13757,#13758,#13759,#13760));
#6270=EDGE_LOOP('',(#13761,#13762,#13763,#13764,#13765,#13766));
#6271=EDGE_LOOP('',(#13767,#13768,#13769,#13770,#13771,#13772));
#6272=EDGE_LOOP('',(#13773,#13774,#13775,#13776,#13777,#13778,#13779,#13780,
#13781,#13782,#13783,#13784,#13785,#13786,#13787,#13788,#13789,#13790,#13791,
#13792));
#6273=EDGE_LOOP('',(#13793,#13794,#13795,#13796));
#6274=EDGE_LOOP('',(#13797,#13798,#13799,#13800));
#6275=EDGE_LOOP('',(#13801,#13802,#13803,#13804,#13805));
#6276=EDGE_LOOP('',(#13806,#13807,#13808,#13809,#13810));
#6277=EDGE_LOOP('',(#13811,#13812,#13813,#13814));
#6278=EDGE_LOOP('',(#13815,#13816,#13817,#13818));
#6279=EDGE_LOOP('',(#13819,#13820));
#6280=EDGE_LOOP('',(#13821,#13822));
#6281=EDGE_LOOP('',(#13823,#13824,#13825,#13826,#13827));
#6282=EDGE_LOOP('',(#13828,#13829));
#6283=EDGE_LOOP('',(#13830,#13831,#13832,#13833,#13834,#13835,#13836,#13837));
#6284=EDGE_LOOP('',(#13838,#13839));
#6285=EDGE_LOOP('',(#13840,#13841,#13842,#13843,#13844));
#6286=EDGE_LOOP('',(#13845,#13846));
#6287=EDGE_LOOP('',(#13847,#13848,#13849,#13850,#13851));
#6288=EDGE_LOOP('',(#13852,#13853));
#6289=EDGE_LOOP('',(#13854,#13855));
#6290=EDGE_LOOP('',(#13856,#13857,#13858,#13859,#13860,#13861));
#6291=EDGE_LOOP('',(#13862,#13863,#13864,#13865,#13866,#13867));
#6292=EDGE_LOOP('',(#13868,#13869,#13870,#13871,#13872,#13873));
#6293=EDGE_LOOP('',(#13874,#13875,#13876,#13877,#13878,#13879));
#6294=EDGE_LOOP('',(#13880,#13881,#13882,#13883,#13884,#13885,#13886,#13887,
#13888,#13889,#13890,#13891,#13892,#13893,#13894,#13895));
#6295=EDGE_LOOP('',(#13896,#13897,#13898,#13899,#13900,#13901));
#6296=EDGE_LOOP('',(#13902,#13903,#13904,#13905,#13906,#13907));
#6297=EDGE_LOOP('',(#13908,#13909,#13910,#13911));
#6298=EDGE_LOOP('',(#13912,#13913,#13914,#13915));
#6299=EDGE_LOOP('',(#13916,#13917,#13918,#13919));
#6300=EDGE_LOOP('',(#13920,#13921,#13922,#13923));
#6301=EDGE_LOOP('',(#13924,#13925,#13926,#13927));
#6302=EDGE_LOOP('',(#13928,#13929,#13930,#13931));
#6303=EDGE_LOOP('',(#13932,#13933,#13934,#13935,#13936));
#6304=EDGE_LOOP('',(#13937,#13938,#13939,#13940));
#6305=EDGE_LOOP('',(#13941,#13942,#13943,#13944,#13945));
#6306=EDGE_LOOP('',(#13946,#13947,#13948,#13949));
#6307=EDGE_LOOP('',(#13950,#13951,#13952,#13953));
#6308=EDGE_LOOP('',(#13954,#13955,#13956,#13957));
#6309=EDGE_LOOP('',(#13958,#13959,#13960,#13961));
#6310=EDGE_LOOP('',(#13962,#13963,#13964,#13965));
#6311=EDGE_LOOP('',(#13966,#13967,#13968,#13969));
#6312=EDGE_LOOP('',(#13970,#13971,#13972,#13973,#13974));
#6313=EDGE_LOOP('',(#13975,#13976,#13977,#13978));
#6314=EDGE_LOOP('',(#13979,#13980,#13981,#13982,#13983));
#6315=EDGE_LOOP('',(#13984,#13985,#13986,#13987));
#6316=EDGE_LOOP('',(#13988,#13989,#13990,#13991));
#6317=EDGE_LOOP('',(#13992,#13993,#13994,#13995));
#6318=EDGE_LOOP('',(#13996,#13997,#13998,#13999));
#6319=EDGE_LOOP('',(#14000,#14001,#14002,#14003));
#6320=EDGE_LOOP('',(#14004,#14005,#14006,#14007));
#6321=EDGE_LOOP('',(#14008,#14009,#14010,#14011,#14012));
#6322=EDGE_LOOP('',(#14013,#14014,#14015,#14016));
#6323=EDGE_LOOP('',(#14017,#14018,#14019,#14020,#14021));
#6324=EDGE_LOOP('',(#14022,#14023,#14024,#14025,#14026,#14027,#14028,#14029,
#14030,#14031,#14032,#14033,#14034,#14035,#14036,#14037));
#6325=EDGE_LOOP('',(#14038,#14039,#14040,#14041));
#6326=EDGE_LOOP('',(#14042,#14043,#14044,#14045));
#6327=EDGE_LOOP('',(#14046,#14047,#14048,#14049));
#6328=EDGE_LOOP('',(#14050,#14051,#14052,#14053));
#6329=EDGE_LOOP('',(#14054,#14055,#14056,#14057));
#6330=EDGE_LOOP('',(#14058,#14059,#14060,#14061));
#6331=EDGE_LOOP('',(#14062,#14063,#14064,#14065,#14066));
#6332=EDGE_LOOP('',(#14067,#14068,#14069,#14070));
#6333=EDGE_LOOP('',(#14071,#14072,#14073,#14074,#14075));
#6334=EDGE_LOOP('',(#14076,#14077,#14078,#14079));
#6335=EDGE_LOOP('',(#14080,#14081,#14082,#14083));
#6336=EDGE_LOOP('',(#14084,#14085,#14086,#14087));
#6337=EDGE_LOOP('',(#14088,#14089,#14090,#14091));
#6338=EDGE_LOOP('',(#14092,#14093,#14094,#14095));
#6339=EDGE_LOOP('',(#14096,#14097,#14098,#14099));
#6340=EDGE_LOOP('',(#14100,#14101,#14102,#14103));
#6341=EDGE_LOOP('',(#14104,#14105,#14106,#14107));
#6342=EDGE_LOOP('',(#14108,#14109,#14110,#14111));
#6343=EDGE_LOOP('',(#14112,#14113,#14114,#14115));
#6344=EDGE_LOOP('',(#14116,#14117,#14118,#14119));
#6345=EDGE_LOOP('',(#14120,#14121,#14122,#14123));
#6346=EDGE_LOOP('',(#14124,#14125,#14126,#14127));
#6347=EDGE_LOOP('',(#14128,#14129,#14130,#14131));
#6348=EDGE_LOOP('',(#14132,#14133,#14134,#14135));
#6349=EDGE_LOOP('',(#14136,#14137,#14138,#14139));
#6350=EDGE_LOOP('',(#14140,#14141,#14142,#14143));
#6351=EDGE_LOOP('',(#14144,#14145,#14146,#14147));
#6352=EDGE_LOOP('',(#14148,#14149,#14150,#14151));
#6353=EDGE_LOOP('',(#14152,#14153,#14154,#14155));
#6354=EDGE_LOOP('',(#14156,#14157,#14158,#14159));
#6355=EDGE_LOOP('',(#14160,#14161,#14162,#14163));
#6356=EDGE_LOOP('',(#14164,#14165,#14166,#14167));
#6357=EDGE_LOOP('',(#14168,#14169,#14170,#14171));
#6358=EDGE_LOOP('',(#14172,#14173,#14174,#14175));
#6359=EDGE_LOOP('',(#14176,#14177,#14178,#14179));
#6360=EDGE_LOOP('',(#14180,#14181,#14182,#14183));
#6361=EDGE_LOOP('',(#14184,#14185,#14186,#14187));
#6362=EDGE_LOOP('',(#14188,#14189,#14190,#14191));
#6363=EDGE_LOOP('',(#14192,#14193,#14194,#14195,#14196,#14197));
#6364=EDGE_LOOP('',(#14198,#14199,#14200,#14201,#14202,#14203));
#6365=EDGE_LOOP('',(#14204,#14205,#14206,#14207));
#6366=EDGE_LOOP('',(#14208,#14209,#14210,#14211,#14212,#14213));
#6367=EDGE_LOOP('',(#14214,#14215,#14216,#14217,#14218,#14219));
#6368=EDGE_LOOP('',(#14220,#14221,#14222,#14223,#14224,#14225));
#6369=EDGE_LOOP('',(#14226,#14227,#14228,#14229,#14230,#14231));
#6370=EDGE_LOOP('',(#14232,#14233,#14234,#14235));
#6371=EDGE_LOOP('',(#14236,#14237,#14238,#14239,#14240,#14241));
#6372=EDGE_LOOP('',(#14242,#14243,#14244,#14245,#14246,#14247));
#6373=EDGE_LOOP('',(#14248,#14249,#14250,#14251));
#6374=EDGE_LOOP('',(#14252,#14253,#14254,#14255));
#6375=EDGE_LOOP('',(#14256,#14257,#14258,#14259));
#6376=EDGE_LOOP('',(#14260,#14261,#14262,#14263));
#6377=EDGE_LOOP('',(#14264,#14265,#14266,#14267));
#6378=EDGE_LOOP('',(#14268,#14269,#14270,#14271));
#6379=EDGE_LOOP('',(#14272,#14273,#14274,#14275));
#6380=EDGE_LOOP('',(#14276,#14277,#14278,#14279));
#6381=EDGE_LOOP('',(#14280,#14281,#14282,#14283));
#6382=EDGE_LOOP('',(#14284,#14285,#14286,#14287));
#6383=EDGE_LOOP('',(#14288,#14289,#14290,#14291));
#6384=EDGE_LOOP('',(#14292,#14293,#14294,#14295));
#6385=EDGE_LOOP('',(#14296,#14297,#14298,#14299,#14300,#14301,#14302,#14303,
#14304,#14305,#14306,#14307,#14308,#14309,#14310,#14311,#14312,#14313,#14314,
#14315,#14316,#14317,#14318,#14319,#14320,#14321,#14322,#14323,#14324,#14325,
#14326,#14327,#14328,#14329,#14330,#14331,#14332,#14333,#14334,#14335,#14336,
#14337,#14338,#14339,#14340,#14341,#14342,#14343,#14344,#14345,#14346,#14347,
#14348,#14349,#14350,#14351));
#6386=EDGE_LOOP('',(#14352,#14353,#14354,#14355,#14356,#14357,#14358,#14359,
#14360,#14361,#14362,#14363,#14364,#14365,#14366,#14367));
#6387=EDGE_LOOP('',(#14368));
#6388=EDGE_LOOP('',(#14369));
#6389=EDGE_LOOP('',(#14370));
#6390=EDGE_LOOP('',(#14371,#14372,#14373,#14374,#14375,#14376));
#6391=EDGE_LOOP('',(#14377));
#6392=EDGE_LOOP('',(#14378,#14379,#14380,#14381,#14382,#14383));
#6393=EDGE_LOOP('',(#14384,#14385,#14386,#14387));
#6394=EDGE_LOOP('',(#14388,#14389,#14390,#14391,#14392,#14393,#14394,#14395));
#6395=EDGE_LOOP('',(#14396,#14397,#14398,#14399));
#6396=EDGE_LOOP('',(#14400,#14401,#14402,#14403,#14404,#14405,#14406,#14407));
#6397=EDGE_LOOP('',(#14408,#14409,#14410,#14411));
#6398=EDGE_LOOP('',(#14412,#14413,#14414,#14415,#14416,#14417,#14418,#14419));
#6399=EDGE_LOOP('',(#14420,#14421,#14422,#14423));
#6400=EDGE_LOOP('',(#14424,#14425,#14426,#14427,#14428,#14429,#14430,#14431));
#6401=EDGE_LOOP('',(#14432,#14433,#14434,#14435,#14436));
#6402=EDGE_LOOP('',(#14437,#14438,#14439,#14440,#14441,#14442));
#6403=EDGE_LOOP('',(#14443,#14444,#14445,#14446,#14447));
#6404=EDGE_LOOP('',(#14448,#14449,#14450,#14451));
#6405=EDGE_LOOP('',(#14452,#14453));
#6406=EDGE_LOOP('',(#14454,#14455,#14456,#14457,#14458,#14459));
#6407=EDGE_LOOP('',(#14460,#14461,#14462,#14463));
#6408=EDGE_LOOP('',(#14464,#14465));
#6409=EDGE_LOOP('',(#14466,#14467,#14468,#14469,#14470,#14471));
#6410=EDGE_LOOP('',(#14472,#14473,#14474,#14475));
#6411=EDGE_LOOP('',(#14476,#14477));
#6412=EDGE_LOOP('',(#14478,#14479,#14480,#14481,#14482,#14483));
#6413=EDGE_LOOP('',(#14484,#14485,#14486,#14487));
#6414=EDGE_LOOP('',(#14488,#14489));
#6415=EDGE_LOOP('',(#14490,#14491,#14492,#14493,#14494,#14495));
#6416=EDGE_LOOP('',(#14496,#14497,#14498,#14499));
#6417=EDGE_LOOP('',(#14500,#14501));
#6418=EDGE_LOOP('',(#14502,#14503,#14504,#14505,#14506,#14507));
#6419=EDGE_LOOP('',(#14508,#14509));
#6420=EDGE_LOOP('',(#14510,#14511));
#6421=EDGE_LOOP('',(#14512,#14513,#14514,#14515,#14516,#14517));
#6422=EDGE_LOOP('',(#14518,#14519,#14520,#14521,#14522,#14523));
#6423=EDGE_LOOP('',(#14524,#14525));
#6424=EDGE_LOOP('',(#14526,#14527));
#6425=EDGE_LOOP('',(#14528,#14529,#14530,#14531));
#6426=EDGE_LOOP('',(#14532,#14533));
#6427=EDGE_LOOP('',(#14534,#14535,#14536,#14537,#14538,#14539));
#6428=EDGE_LOOP('',(#14540,#14541,#14542,#14543));
#6429=EDGE_LOOP('',(#14544,#14545));
#6430=EDGE_LOOP('',(#14546,#14547,#14548,#14549,#14550,#14551));
#6431=EDGE_LOOP('',(#14552,#14553,#14554,#14555));
#6432=EDGE_LOOP('',(#14556,#14557,#14558,#14559,#14560,#14561,#14562,#14563));
#6433=EDGE_LOOP('',(#14564,#14565));
#6434=EDGE_LOOP('',(#14566,#14567));
#6435=EDGE_LOOP('',(#14568,#14569));
#6436=EDGE_LOOP('',(#14570,#14571,#14572,#14573));
#6437=EDGE_LOOP('',(#14574,#14575));
#6438=EDGE_LOOP('',(#14576,#14577,#14578,#14579,#14580,#14581));
#6439=EDGE_LOOP('',(#14582,#14583,#14584,#14585));
#6440=EDGE_LOOP('',(#14586,#14587));
#6441=EDGE_LOOP('',(#14588,#14589,#14590,#14591,#14592,#14593));
#6442=EDGE_LOOP('',(#14594,#14595,#14596,#14597));
#6443=EDGE_LOOP('',(#14598,#14599));
#6444=EDGE_LOOP('',(#14600,#14601,#14602,#14603,#14604,#14605));
#6445=EDGE_LOOP('',(#14606,#14607,#14608,#14609));
#6446=EDGE_LOOP('',(#14610,#14611));
#6447=EDGE_LOOP('',(#14612,#14613,#14614,#14615,#14616,#14617));
#6448=EDGE_LOOP('',(#14618,#14619,#14620,#14621));
#6449=EDGE_LOOP('',(#14622,#14623,#14624,#14625,#14626));
#6450=EDGE_LOOP('',(#14627,#14628,#14629,#14630,#14631,#14632));
#6451=EDGE_LOOP('',(#14633,#14634,#14635,#14636,#14637,#14638));
#6452=EDGE_LOOP('',(#14639,#14640));
#6453=EDGE_LOOP('',(#14641,#14642,#14643,#14644));
#6454=EDGE_LOOP('',(#14645,#14646,#14647,#14648));
#6455=EDGE_LOOP('',(#14649,#14650));
#6456=EDGE_LOOP('',(#14651,#14652,#14653,#14654,#14655,#14656));
#6457=EDGE_LOOP('',(#14657,#14658,#14659,#14660));
#6458=EDGE_LOOP('',(#14661,#14662));
#6459=EDGE_LOOP('',(#14663,#14664,#14665,#14666,#14667,#14668));
#6460=EDGE_LOOP('',(#14669,#14670,#14671,#14672));
#6461=EDGE_LOOP('',(#14673,#14674));
#6462=EDGE_LOOP('',(#14675,#14676,#14677,#14678,#14679,#14680));
#6463=EDGE_LOOP('',(#14681,#14682,#14683,#14684));
#6464=EDGE_LOOP('',(#14685,#14686,#14687,#14688,#14689,#14690));
#6465=EDGE_LOOP('',(#14691,#14692,#14693,#14694,#14695,#14696,#14697,#14698));
#6466=EDGE_LOOP('',(#14699,#14700,#14701,#14702,#14703,#14704,#14705,#14706));
#6467=EDGE_LOOP('',(#14707,#14708,#14709,#14710));
#6468=EDGE_LOOP('',(#14711,#14712,#14713,#14714));
#6469=EDGE_LOOP('',(#14715,#14716,#14717,#14718));
#6470=EDGE_LOOP('',(#14719,#14720,#14721,#14722,#14723,#14724,#14725,#14726,
#14727,#14728,#14729,#14730,#14731,#14732,#14733,#14734,#14735,#14736,#14737,
#14738));
#6471=EDGE_LOOP('',(#14739,#14740,#14741,#14742));
#6472=EDGE_LOOP('',(#14743,#14744,#14745,#14746));
#6473=EDGE_LOOP('',(#14747,#14748,#14749,#14750));
#6474=EDGE_LOOP('',(#14751,#14752,#14753,#14754));
#6475=EDGE_LOOP('',(#14755,#14756,#14757,#14758));
#6476=EDGE_LOOP('',(#14759,#14760,#14761,#14762));
#6477=EDGE_LOOP('',(#14763,#14764,#14765,#14766,#14767,#14768,#14769,#14770,
#14771,#14772,#14773,#14774,#14775,#14776,#14777,#14778,#14779,#14780,#14781,
#14782));
#6478=EDGE_LOOP('',(#14783,#14784,#14785,#14786));
#6479=EDGE_LOOP('',(#14787,#14788,#14789,#14790));
#6480=EDGE_LOOP('',(#14791,#14792,#14793,#14794,#14795));
#6481=EDGE_LOOP('',(#14796,#14797,#14798,#14799,#14800,#14801,#14802,#14803,
#14804,#14805,#14806,#14807,#14808,#14809,#14810,#14811,#14812,#14813,#14814,
#14815));
#6482=EDGE_LOOP('',(#14816,#14817,#14818,#14819));
#6483=EDGE_LOOP('',(#14820,#14821,#14822,#14823));
#6484=EDGE_LOOP('',(#14824));
#6485=EDGE_LOOP('',(#14825));
#6486=EDGE_LOOP('',(#14826,#14827,#14828,#14829,#14830,#14831));
#6487=EDGE_LOOP('',(#14832,#14833,#14834,#14835));
#6488=EDGE_LOOP('',(#14836,#14837,#14838,#14839,#14840,#14841));
#6489=EDGE_LOOP('',(#14842,#14843,#14844,#14845,#14846,#14847));
#6490=EDGE_LOOP('',(#14848,#14849,#14850,#14851,#14852,#14853));
#6491=EDGE_LOOP('',(#14854,#14855,#14856,#14857));
#6492=EDGE_LOOP('',(#14858,#14859,#14860,#14861));
#6493=EDGE_LOOP('',(#14862,#14863,#14864,#14865));
#6494=EDGE_LOOP('',(#14866,#14867,#14868,#14869));
#6495=EDGE_LOOP('',(#14870,#14871,#14872,#14873));
#6496=EDGE_LOOP('',(#14874,#14875,#14876,#14877));
#6497=EDGE_LOOP('',(#14878,#14879,#14880,#14881));
#6498=EDGE_LOOP('',(#14882,#14883,#14884,#14885));
#6499=EDGE_LOOP('',(#14886,#14887,#14888,#14889));
#6500=EDGE_LOOP('',(#14890,#14891,#14892,#14893));
#6501=EDGE_LOOP('',(#14894,#14895,#14896,#14897));
#6502=EDGE_LOOP('',(#14898,#14899,#14900,#14901));
#6503=EDGE_LOOP('',(#14902,#14903,#14904,#14905));
#6504=EDGE_LOOP('',(#14906,#14907,#14908,#14909,#14910,#14911,#14912,#14913,
#14914,#14915,#14916,#14917,#14918,#14919,#14920,#14921,#14922,#14923,#14924,
#14925,#14926,#14927,#14928,#14929));
#6505=EDGE_LOOP('',(#14930,#14931,#14932,#14933,#14934,#14935,#14936,#14937,
#14938,#14939,#14940,#14941,#14942,#14943,#14944,#14945));
#6506=EDGE_LOOP('',(#14946,#14947,#14948,#14949,#14950,#14951));
#6507=EDGE_LOOP('',(#14952,#14953,#14954,#14955,#14956,#14957));
#6508=EDGE_LOOP('',(#14958,#14959,#14960,#14961));
#6509=EDGE_LOOP('',(#14962,#14963,#14964,#14965));
#6510=EDGE_LOOP('',(#14966,#14967,#14968,#14969));
#6511=EDGE_LOOP('',(#14970,#14971,#14972,#14973));
#6512=EDGE_LOOP('',(#14974,#14975,#14976,#14977));
#6513=EDGE_LOOP('',(#14978,#14979,#14980,#14981));
#6514=EDGE_LOOP('',(#14982,#14983,#14984,#14985,#14986,#14987));
#6515=EDGE_LOOP('',(#14988,#14989,#14990,#14991));
#6516=EDGE_LOOP('',(#14992,#14993,#14994,#14995));
#6517=EDGE_LOOP('',(#14996,#14997,#14998,#14999));
#6518=EDGE_LOOP('',(#15000,#15001,#15002,#15003));
#6519=EDGE_LOOP('',(#15004,#15005,#15006,#15007));
#6520=EDGE_LOOP('',(#15008,#15009,#15010,#15011,#15012,#15013));
#6521=EDGE_LOOP('',(#15014,#15015,#15016,#15017));
#6522=EDGE_LOOP('',(#15018,#15019,#15020,#15021));
#6523=EDGE_LOOP('',(#15022,#15023,#15024,#15025));
#6524=EDGE_LOOP('',(#15026,#15027,#15028,#15029));
#6525=EDGE_LOOP('',(#15030,#15031,#15032,#15033,#15034,#15035));
#6526=EDGE_LOOP('',(#15036,#15037,#15038,#15039));
#6527=EDGE_LOOP('',(#15040,#15041,#15042,#15043));
#6528=EDGE_LOOP('',(#15044,#15045,#15046,#15047));
#6529=EDGE_LOOP('',(#15048,#15049,#15050,#15051));
#6530=EDGE_LOOP('',(#15052,#15053,#15054,#15055));
#6531=EDGE_LOOP('',(#15056,#15057,#15058,#15059,#15060,#15061));
#6532=EDGE_LOOP('',(#15062,#15063,#15064,#15065));
#6533=EDGE_LOOP('',(#15066,#15067,#15068,#15069));
#6534=EDGE_LOOP('',(#15070,#15071,#15072,#15073));
#6535=EDGE_LOOP('',(#15074,#15075,#15076,#15077));
#6536=EDGE_LOOP('',(#15078,#15079,#15080,#15081));
#6537=EDGE_LOOP('',(#15082,#15083,#15084,#15085));
#6538=EDGE_LOOP('',(#15086,#15087,#15088,#15089));
#6539=EDGE_LOOP('',(#15090,#15091,#15092,#15093));
#6540=EDGE_LOOP('',(#15094,#15095,#15096,#15097));
#6541=EDGE_LOOP('',(#15098,#15099,#15100,#15101));
#6542=EDGE_LOOP('',(#15102,#15103,#15104,#15105));
#6543=EDGE_LOOP('',(#15106,#15107,#15108,#15109));
#6544=EDGE_LOOP('',(#15110,#15111,#15112,#15113));
#6545=EDGE_LOOP('',(#15114,#15115,#15116,#15117));
#6546=EDGE_LOOP('',(#15118,#15119,#15120,#15121));
#6547=EDGE_LOOP('',(#15122,#15123,#15124,#15125));
#6548=EDGE_LOOP('',(#15126,#15127,#15128,#15129));
#6549=EDGE_LOOP('',(#15130,#15131,#15132,#15133,#15134,#15135,#15136,#15137));
#6550=EDGE_LOOP('',(#15138,#15139,#15140,#15141));
#6551=EDGE_LOOP('',(#15142,#15143,#15144,#15145,#15146,#15147));
#6552=EDGE_LOOP('',(#15148,#15149,#15150,#15151));
#6553=EDGE_LOOP('',(#15152,#15153,#15154,#15155));
#6554=EDGE_LOOP('',(#15156,#15157,#15158,#15159));
#6555=EDGE_LOOP('',(#15160,#15161,#15162,#15163));
#6556=EDGE_LOOP('',(#15164,#15165,#15166,#15167,#15168,#15169,#15170,#15171,
#15172,#15173,#15174,#15175,#15176,#15177,#15178,#15179,#15180,#15181,#15182,
#15183,#15184,#15185,#15186,#15187));
#6557=EDGE_LOOP('',(#15188,#15189,#15190,#15191,#15192,#15193,#15194,#15195,
#15196,#15197,#15198,#15199,#15200,#15201,#15202,#15203));
#6558=EDGE_LOOP('',(#15204,#15205,#15206,#15207));
#6559=EDGE_LOOP('',(#15208));
#6560=EDGE_LOOP('',(#15209,#15210,#15211,#15212,#15213,#15214));
#6561=EDGE_LOOP('',(#15215));
#6562=EDGE_LOOP('',(#15216,#15217,#15218,#15219,#15220,#15221));
#6563=EDGE_LOOP('',(#15222,#15223,#15224,#15225,#15226,#15227));
#6564=EDGE_LOOP('',(#15228,#15229,#15230,#15231,#15232,#15233));
#6565=EDGE_LOOP('',(#15234,#15235,#15236,#15237,#15238,#15239,#15240,#15241,
#15242,#15243));
#6566=EDGE_LOOP('',(#15244,#15245,#15246,#15247));
#6567=EDGE_LOOP('',(#15248,#15249,#15250,#15251,#15252,#15253,#15254,#15255));
#6568=EDGE_LOOP('',(#15256,#15257,#15258,#15259,#15260,#15261));
#6569=EDGE_LOOP('',(#15262));
#6570=EDGE_LOOP('',(#15263,#15264,#15265,#15266,#15267));
#6571=EDGE_LOOP('',(#15268,#15269,#15270,#15271,#15272,#15273));
#6572=EDGE_LOOP('',(#15274,#15275,#15276,#15277,#15278,#15279));
#6573=EDGE_LOOP('',(#15280,#15281,#15282,#15283,#15284,#15285));
#6574=EDGE_LOOP('',(#15286,#15287,#15288,#15289,#15290,#15291,#15292,#15293));
#6575=EDGE_LOOP('',(#15294,#15295,#15296,#15297,#15298));
#6576=EDGE_LOOP('',(#15299,#15300,#15301,#15302));
#6577=EDGE_LOOP('',(#15303,#15304,#15305,#15306,#15307,#15308));
#6578=EDGE_LOOP('',(#15309,#15310,#15311,#15312,#15313,#15314));
#6579=EDGE_LOOP('',(#15315));
#6580=EDGE_LOOP('',(#15316,#15317,#15318,#15319,#15320,#15321));
#6581=EDGE_LOOP('',(#15322,#15323,#15324,#15325,#15326,#15327,#15328,#15329,
#15330,#15331));
#6582=EDGE_LOOP('',(#15332,#15333,#15334,#15335));
#6583=EDGE_LOOP('',(#15336,#15337,#15338,#15339,#15340,#15341));
#6584=EDGE_LOOP('',(#15342,#15343,#15344,#15345,#15346,#15347));
#6585=EDGE_LOOP('',(#15348));
#6586=EDGE_LOOP('',(#15349,#15350,#15351,#15352));
#6587=EDGE_LOOP('',(#15353,#15354,#15355,#15356,#15357,#15358));
#6588=EDGE_LOOP('',(#15359));
#6589=EDGE_LOOP('',(#15360,#15361,#15362,#15363,#15364,#15365));
#6590=EDGE_LOOP('',(#15366,#15367,#15368,#15369,#15370,#15371,#15372,#15373,
#15374,#15375));
#6591=EDGE_LOOP('',(#15376,#15377,#15378,#15379,#15380,#15381));
#6592=EDGE_LOOP('',(#15382,#15383,#15384,#15385));
#6593=EDGE_LOOP('',(#15386));
#6594=EDGE_LOOP('',(#15387));
#6595=EDGE_LOOP('',(#15388,#15389,#15390,#15391,#15392,#15393));
#6596=EDGE_LOOP('',(#15394));
#6597=EDGE_LOOP('',(#15395,#15396,#15397,#15398));
#6598=EDGE_LOOP('',(#15399,#15400,#15401,#15402,#15403,#15404,#15405,#15406));
#6599=EDGE_LOOP('',(#15407,#15408,#15409,#15410));
#6600=EDGE_LOOP('',(#15411,#15412,#15413,#15414));
#6601=EDGE_LOOP('',(#15415,#15416,#15417,#15418));
#6602=EDGE_LOOP('',(#15419,#15420,#15421,#15422));
#6603=EDGE_LOOP('',(#15423,#15424,#15425,#15426));
#6604=EDGE_LOOP('',(#15427,#15428,#15429,#15430,#15431,#15432,#15433,#15434));
#6605=EDGE_LOOP('',(#15435,#15436,#15437,#15438,#15439,#15440));
#6606=EDGE_LOOP('',(#15441));
#6607=EDGE_LOOP('',(#15442,#15443,#15444,#15445));
#6608=EDGE_LOOP('',(#15446,#15447,#15448,#15449,#15450,#15451,#15452,#15453));
#6609=EDGE_LOOP('',(#15454,#15455,#15456,#15457));
#6610=EDGE_LOOP('',(#15458,#15459,#15460,#15461,#15462,#15463));
#6611=EDGE_LOOP('',(#15464,#15465,#15466,#15467));
#6612=EDGE_LOOP('',(#15468,#15469,#15470,#15471,#15472,#15473));
#6613=EDGE_LOOP('',(#15474,#15475,#15476,#15477));
#6614=EDGE_LOOP('',(#15478,#15479,#15480,#15481,#15482,#15483,#15484,#15485));
#6615=EDGE_LOOP('',(#15486,#15487,#15488,#15489,#15490,#15491));
#6616=EDGE_LOOP('',(#15492));
#6617=EDGE_LOOP('',(#15493,#15494,#15495,#15496));
#6618=EDGE_LOOP('',(#15497,#15498,#15499,#15500,#15501,#15502,#15503,#15504));
#6619=EDGE_LOOP('',(#15505,#15506,#15507,#15508));
#6620=EDGE_LOOP('',(#15509,#15510,#15511,#15512));
#6621=EDGE_LOOP('',(#15513,#15514,#15515,#15516));
#6622=EDGE_LOOP('',(#15517,#15518,#15519,#15520));
#6623=EDGE_LOOP('',(#15521,#15522,#15523,#15524));
#6624=EDGE_LOOP('',(#15525,#15526,#15527,#15528,#15529,#15530,#15531,#15532));
#6625=EDGE_LOOP('',(#15533,#15534,#15535,#15536,#15537,#15538));
#6626=EDGE_LOOP('',(#15539));
#6627=EDGE_LOOP('',(#15540,#15541,#15542,#15543));
#6628=EDGE_LOOP('',(#15544,#15545,#15546,#15547,#15548,#15549,#15550,#15551));
#6629=EDGE_LOOP('',(#15552,#15553,#15554,#15555));
#6630=EDGE_LOOP('',(#15556,#15557,#15558,#15559));
#6631=EDGE_LOOP('',(#15560,#15561,#15562,#15563));
#6632=EDGE_LOOP('',(#15564,#15565,#15566,#15567));
#6633=EDGE_LOOP('',(#15568,#15569,#15570,#15571));
#6634=EDGE_LOOP('',(#15572,#15573,#15574,#15575,#15576,#15577,#15578,#15579));
#6635=EDGE_LOOP('',(#15580,#15581,#15582,#15583));
#6636=EDGE_LOOP('',(#15584,#15585,#15586,#15587));
#6637=EDGE_LOOP('',(#15588,#15589,#15590,#15591));
#6638=EDGE_LOOP('',(#15592,#15593,#15594,#15595));
#6639=EDGE_LOOP('',(#15596,#15597,#15598,#15599));
#6640=EDGE_LOOP('',(#15600,#15601,#15602,#15603));
#6641=EDGE_LOOP('',(#15604));
#6642=EDGE_LOOP('',(#15605));
#6643=EDGE_LOOP('',(#15606));
#6644=EDGE_LOOP('',(#15607));
#6645=EDGE_LOOP('',(#15608,#15609,#15610,#15611));
#6646=EDGE_LOOP('',(#15612,#15613,#15614,#15615,#15616));
#6647=EDGE_LOOP('',(#15617,#15618,#15619,#15620));
#6648=EDGE_LOOP('',(#15621,#15622,#15623,#15624,#15625));
#6649=EDGE_LOOP('',(#15626));
#6650=EDGE_LOOP('',(#15627));
#6651=EDGE_LOOP('',(#15628));
#6652=EDGE_LOOP('',(#15629));
#6653=EDGE_LOOP('',(#15630,#15631,#15632,#15633,#15634,#15635));
#6654=EDGE_LOOP('',(#15636,#15637,#15638,#15639,#15640,#15641,#15642,#15643));
#6655=EDGE_LOOP('',(#15644,#15645,#15646,#15647,#15648,#15649));
#6656=EDGE_LOOP('',(#15650,#15651,#15652,#15653,#15654,#15655,#15656,#15657,
#15658,#15659));
#6657=EDGE_LOOP('',(#15660,#15661,#15662,#15663,#15664,#15665));
#6658=EDGE_LOOP('',(#15666,#15667,#15668,#15669,#15670,#15671,#15672,#15673));
#6659=EDGE_LOOP('',(#15674,#15675,#15676,#15677,#15678,#15679));
#6660=EDGE_LOOP('',(#15680,#15681,#15682,#15683,#15684,#15685,#15686,#15687,
#15688,#15689));
#6661=EDGE_LOOP('',(#15690,#15691,#15692,#15693,#15694,#15695));
#6662=EDGE_LOOP('',(#15696,#15697,#15698,#15699,#15700,#15701,#15702,#15703));
#6663=EDGE_LOOP('',(#15704,#15705,#15706,#15707,#15708,#15709));
#6664=EDGE_LOOP('',(#15710,#15711,#15712,#15713,#15714,#15715,#15716,#15717,
#15718,#15719));
#6665=EDGE_LOOP('',(#15720,#15721,#15722,#15723,#15724,#15725));
#6666=EDGE_LOOP('',(#15726,#15727,#15728,#15729,#15730,#15731,#15732,#15733));
#6667=EDGE_LOOP('',(#15734,#15735,#15736,#15737,#15738,#15739));
#6668=EDGE_LOOP('',(#15740,#15741,#15742,#15743,#15744,#15745,#15746,#15747,
#15748,#15749));
#6669=EDGE_LOOP('',(#15750));
#6670=EDGE_LOOP('',(#15751,#15752,#15753,#15754,#15755,#15756));
#6671=EDGE_LOOP('',(#15757,#15758,#15759,#15760,#15761,#15762));
#6672=EDGE_LOOP('',(#15763,#15764,#15765,#15766));
#6673=EDGE_LOOP('',(#15767,#15768,#15769,#15770));
#6674=EDGE_LOOP('',(#15771,#15772,#15773,#15774));
#6675=EDGE_LOOP('',(#15775,#15776,#15777,#15778,#15779,#15780,#15781,#15782,
#15783));
#6676=EDGE_LOOP('',(#15784,#15785,#15786,#15787));
#6677=EDGE_LOOP('',(#15788,#15789,#15790,#15791));
#6678=EDGE_LOOP('',(#15792,#15793,#15794,#15795));
#6679=EDGE_LOOP('',(#15796,#15797,#15798,#15799));
#6680=EDGE_LOOP('',(#15800,#15801,#15802,#15803));
#6681=EDGE_LOOP('',(#15804,#15805,#15806,#15807));
#6682=EDGE_LOOP('',(#15808,#15809,#15810,#15811,#15812,#15813,#15814,#15815));
#6683=EDGE_LOOP('',(#15816,#15817,#15818,#15819));
#6684=EDGE_LOOP('',(#15820,#15821,#15822,#15823));
#6685=EDGE_LOOP('',(#15824,#15825,#15826,#15827));
#6686=EDGE_LOOP('',(#15828,#15829,#15830,#15831,#15832,#15833,#15834,#15835));
#6687=EDGE_LOOP('',(#15836,#15837,#15838,#15839,#15840,#15841,#15842,#15843));
#6688=EDGE_LOOP('',(#15844));
#6689=EDGE_LOOP('',(#15845,#15846,#15847,#15848));
#6690=EDGE_LOOP('',(#15849,#15850,#15851,#15852));
#6691=EDGE_LOOP('',(#15853,#15854,#15855,#15856,#15857,#15858,#15859,#15860));
#6692=EDGE_LOOP('',(#15861));
#6693=EDGE_LOOP('',(#15862,#15863,#15864,#15865,#15866,#15867));
#6694=EDGE_LOOP('',(#15868,#15869,#15870,#15871));
#6695=EDGE_LOOP('',(#15872,#15873,#15874,#15875));
#6696=EDGE_LOOP('',(#15876,#15877,#15878,#15879));
#6697=EDGE_LOOP('',(#15880,#15881,#15882,#15883));
#6698=EDGE_LOOP('',(#15884,#15885,#15886,#15887));
#6699=EDGE_LOOP('',(#15888,#15889,#15890,#15891));
#6700=EDGE_LOOP('',(#15892,#15893,#15894,#15895));
#6701=EDGE_LOOP('',(#15896,#15897,#15898,#15899,#15900,#15901));
#6702=EDGE_LOOP('',(#15902,#15903,#15904,#15905));
#6703=EDGE_LOOP('',(#15906));
#6704=EDGE_LOOP('',(#15907));
#6705=EDGE_LOOP('',(#15908));
#6706=EDGE_LOOP('',(#15909));
#6707=EDGE_LOOP('',(#15910));
#6708=EDGE_LOOP('',(#15911));
#6709=EDGE_LOOP('',(#15912));
#6710=EDGE_LOOP('',(#15913));
#6711=EDGE_LOOP('',(#15914));
#6712=EDGE_LOOP('',(#15915));
#6713=EDGE_LOOP('',(#15916,#15917));
#6714=EDGE_LOOP('',(#15918,#15919,#15920,#15921,#15922));
#6715=EDGE_LOOP('',(#15923,#15924,#15925,#15926,#15927,#15928));
#6716=EDGE_LOOP('',(#15929,#15930,#15931,#15932,#15933,#15934));
#6717=EDGE_LOOP('',(#15935,#15936,#15937,#15938,#15939,#15940));
#6718=EDGE_LOOP('',(#15941,#15942,#15943));
#6719=EDGE_LOOP('',(#15944,#15945,#15946,#15947));
#6720=EDGE_LOOP('',(#15948,#15949,#15950));
#6721=EDGE_LOOP('',(#15951,#15952,#15953));
#6722=EDGE_LOOP('',(#15954,#15955,#15956,#15957));
#6723=EDGE_LOOP('',(#15958,#15959,#15960));
#6724=EDGE_LOOP('',(#15961,#15962,#15963,#15964));
#6725=EDGE_LOOP('',(#15965,#15966,#15967));
#6726=EDGE_LOOP('',(#15968,#15969,#15970,#15971));
#6727=EDGE_LOOP('',(#15972,#15973,#15974));
#6728=EDGE_LOOP('',(#15975,#15976,#15977));
#6729=EDGE_LOOP('',(#15978,#15979,#15980,#15981));
#6730=EDGE_LOOP('',(#15982,#15983,#15984));
#6731=EDGE_LOOP('',(#15985,#15986,#15987,#15988));
#6732=EDGE_LOOP('',(#15989,#15990,#15991,#15992));
#6733=EDGE_LOOP('',(#15993,#15994,#15995,#15996));
#6734=EDGE_LOOP('',(#15997,#15998,#15999,#16000));
#6735=EDGE_LOOP('',(#16001,#16002,#16003,#16004));
#6736=EDGE_LOOP('',(#16005,#16006,#16007,#16008));
#6737=EDGE_LOOP('',(#16009,#16010,#16011,#16012,#16013));
#6738=EDGE_LOOP('',(#16014,#16015,#16016));
#6739=EDGE_LOOP('',(#16017,#16018,#16019,#16020,#16021,#16022));
#6740=EDGE_LOOP('',(#16023,#16024,#16025,#16026,#16027,#16028));
#6741=EDGE_LOOP('',(#16029,#16030,#16031));
#6742=EDGE_LOOP('',(#16032,#16033,#16034,#16035,#16036,#16037));
#6743=EDGE_LOOP('',(#16038,#16039,#16040,#16041,#16042,#16043));
#6744=EDGE_LOOP('',(#16044,#16045,#16046,#16047,#16048,#16049));
#6745=EDGE_LOOP('',(#16050,#16051,#16052,#16053,#16054,#16055));
#6746=EDGE_LOOP('',(#16056,#16057,#16058,#16059));
#6747=EDGE_LOOP('',(#16060,#16061,#16062,#16063));
#6748=EDGE_LOOP('',(#16064,#16065,#16066,#16067));
#6749=EDGE_LOOP('',(#16068,#16069,#16070,#16071));
#6750=EDGE_LOOP('',(#16072,#16073,#16074,#16075,#16076,#16077));
#6751=EDGE_LOOP('',(#16078,#16079,#16080,#16081,#16082,#16083));
#6752=EDGE_LOOP('',(#16084,#16085,#16086,#16087));
#6753=EDGE_LOOP('',(#16088,#16089,#16090,#16091));
#6754=EDGE_LOOP('',(#16092,#16093,#16094,#16095));
#6755=EDGE_LOOP('',(#16096,#16097,#16098,#16099));
#6756=EDGE_LOOP('',(#16100,#16101,#16102,#16103));
#6757=EDGE_LOOP('',(#16104,#16105,#16106,#16107));
#6758=EDGE_LOOP('',(#16108,#16109,#16110));
#6759=EDGE_LOOP('',(#16111,#16112,#16113,#16114));
#6760=EDGE_LOOP('',(#16115,#16116,#16117,#16118,#16119));
#6761=EDGE_LOOP('',(#16120,#16121,#16122,#16123));
#6762=EDGE_LOOP('',(#16124,#16125,#16126,#16127));
#6763=EDGE_LOOP('',(#16128,#16129,#16130,#16131));
#6764=EDGE_LOOP('',(#16132,#16133,#16134,#16135));
#6765=EDGE_LOOP('',(#16136,#16137,#16138,#16139));
#6766=EDGE_LOOP('',(#16140,#16141,#16142,#16143));
#6767=EDGE_LOOP('',(#16144,#16145,#16146,#16147));
#6768=EDGE_LOOP('',(#16148,#16149,#16150,#16151,#16152));
#6769=EDGE_LOOP('',(#16153,#16154,#16155,#16156));
#6770=EDGE_LOOP('',(#16157,#16158,#16159,#16160));
#6771=EDGE_LOOP('',(#16161,#16162,#16163,#16164));
#6772=EDGE_LOOP('',(#16165,#16166,#16167,#16168));
#6773=EDGE_LOOP('',(#16169,#16170,#16171,#16172));
#6774=EDGE_LOOP('',(#16173,#16174,#16175,#16176));
#6775=EDGE_LOOP('',(#16177,#16178,#16179,#16180));
#6776=EDGE_LOOP('',(#16181,#16182,#16183,#16184,#16185,#16186,#16187,#16188,
#16189,#16190,#16191,#16192,#16193,#16194,#16195,#16196,#16197,#16198));
#6777=EDGE_LOOP('',(#16199,#16200,#16201,#16202,#16203,#16204,#16205,#16206,
#16207,#16208,#16209,#16210,#16211,#16212,#16213,#16214,#16215,#16216,#16217,
#16218));
#6778=EDGE_LOOP('',(#16219,#16220,#16221,#16222,#16223,#16224));
#6779=EDGE_LOOP('',(#16225,#16226,#16227));
#6780=EDGE_LOOP('',(#16228,#16229,#16230,#16231,#16232,#16233));
#6781=EDGE_LOOP('',(#16234,#16235,#16236,#16237,#16238,#16239));
#6782=EDGE_LOOP('',(#16240,#16241,#16242));
#6783=EDGE_LOOP('',(#16243,#16244,#16245,#16246,#16247));
#6784=EDGE_LOOP('',(#16248,#16249,#16250,#16251,#16252,#16253));
#6785=EDGE_LOOP('',(#16254,#16255,#16256,#16257,#16258,#16259));
#6786=EDGE_LOOP('',(#16260,#16261,#16262,#16263));
#6787=EDGE_LOOP('',(#16264,#16265,#16266,#16267,#16268,#16269,#16270,#16271));
#6788=EDGE_LOOP('',(#16272,#16273,#16274));
#6789=EDGE_LOOP('',(#16275,#16276,#16277));
#6790=EDGE_LOOP('',(#16278,#16279,#16280,#16281,#16282,#16283,#16284,#16285));
#6791=EDGE_LOOP('',(#16286,#16287,#16288));
#6792=EDGE_LOOP('',(#16289,#16290,#16291,#16292));
#6793=EDGE_LOOP('',(#16293,#16294,#16295,#16296,#16297));
#6794=EDGE_LOOP('',(#16298,#16299,#16300,#16301,#16302,#16303,#16304,#16305,
#16306,#16307,#16308,#16309,#16310,#16311,#16312,#16313,#16314,#16315,#16316,
#16317,#16318,#16319,#16320,#16321,#16322,#16323,#16324,#16325,#16326));
#6795=EDGE_LOOP('',(#16327,#16328,#16329,#16330));
#6796=EDGE_LOOP('',(#16331,#16332,#16333,#16334));
#6797=EDGE_LOOP('',(#16335,#16336,#16337,#16338));
#6798=EDGE_LOOP('',(#16339,#16340,#16341,#16342));
#6799=EDGE_LOOP('',(#16343,#16344,#16345,#16346));
#6800=EDGE_LOOP('',(#16347,#16348,#16349,#16350));
#6801=EDGE_LOOP('',(#16351,#16352,#16353));
#6802=EDGE_LOOP('',(#16354,#16355,#16356));
#6803=EDGE_LOOP('',(#16357,#16358,#16359,#16360));
#6804=EDGE_LOOP('',(#16361,#16362,#16363,#16364,#16365));
#6805=EDGE_LOOP('',(#16366,#16367,#16368,#16369));
#6806=EDGE_LOOP('',(#16370,#16371,#16372,#16373));
#6807=EDGE_LOOP('',(#16374,#16375,#16376,#16377));
#6808=EDGE_LOOP('',(#16378,#16379,#16380,#16381));
#6809=EDGE_LOOP('',(#16382,#16383,#16384,#16385));
#6810=EDGE_LOOP('',(#16386,#16387,#16388,#16389));
#6811=EDGE_LOOP('',(#16390,#16391,#16392,#16393));
#6812=EDGE_LOOP('',(#16394,#16395,#16396,#16397));
#6813=EDGE_LOOP('',(#16398,#16399,#16400,#16401));
#6814=EDGE_LOOP('',(#16402,#16403,#16404,#16405));
#6815=EDGE_LOOP('',(#16406,#16407,#16408,#16409));
#6816=EDGE_LOOP('',(#16410,#16411,#16412,#16413));
#6817=EDGE_LOOP('',(#16414));
#6818=EDGE_LOOP('',(#16415));
#6819=EDGE_LOOP('',(#16416,#16417,#16418,#16419,#16420,#16421));
#6820=EDGE_LOOP('',(#16422));
#6821=EDGE_LOOP('',(#16423,#16424,#16425,#16426));
#6822=EDGE_LOOP('',(#16427));
#6823=EDGE_LOOP('',(#16428));
#6824=EDGE_LOOP('',(#16429));
#6825=EDGE_LOOP('',(#16430));
#6826=EDGE_LOOP('',(#16431,#16432,#16433,#16434,#16435,#16436));
#6827=EDGE_LOOP('',(#16437,#16438,#16439,#16440));
#6828=EDGE_LOOP('',(#16441,#16442,#16443,#16444,#16445,#16446));
#6829=EDGE_LOOP('',(#16447,#16448,#16449,#16450));
#6830=EDGE_LOOP('',(#16451,#16452,#16453,#16454));
#6831=EDGE_LOOP('',(#16455,#16456,#16457,#16458));
#6832=EDGE_LOOP('',(#16459,#16460,#16461,#16462));
#6833=EDGE_LOOP('',(#16463,#16464,#16465,#16466));
#6834=EDGE_LOOP('',(#16467,#16468,#16469,#16470));
#6835=EDGE_LOOP('',(#16471,#16472,#16473,#16474));
#6836=EDGE_LOOP('',(#16475,#16476,#16477,#16478,#16479,#16480));
#6837=EDGE_LOOP('',(#16481,#16482,#16483,#16484));
#6838=EDGE_LOOP('',(#16485,#16486,#16487,#16488));
#6839=EDGE_LOOP('',(#16489,#16490,#16491,#16492,#16493,#16494));
#6840=EDGE_LOOP('',(#16495,#16496,#16497,#16498));
#6841=EDGE_LOOP('',(#16499,#16500,#16501,#16502));
#6842=EDGE_LOOP('',(#16503));
#6843=EDGE_LOOP('',(#16504,#16505,#16506,#16507,#16508,#16509));
#6844=EDGE_LOOP('',(#16510,#16511,#16512,#16513));
#6845=EDGE_LOOP('',(#16514,#16515,#16516,#16517,#16518,#16519,#16520));
#6846=EDGE_LOOP('',(#16521,#16522,#16523,#16524,#16525,#16526));
#6847=EDGE_LOOP('',(#16527,#16528,#16529));
#6848=EDGE_LOOP('',(#16530,#16531,#16532,#16533,#16534,#16535,#16536));
#6849=EDGE_LOOP('',(#16537,#16538,#16539,#16540,#16541,#16542));
#6850=EDGE_LOOP('',(#16543,#16544,#16545,#16546,#16547,#16548,#16549,#16550,
#16551,#16552,#16553,#16554,#16555,#16556,#16557,#16558,#16559,#16560,#16561,
#16562,#16563,#16564,#16565,#16566,#16567,#16568,#16569,#16570,#16571));
#6851=EDGE_LOOP('',(#16572,#16573,#16574));
#6852=EDGE_LOOP('',(#16575,#16576,#16577,#16578));
#6853=EDGE_LOOP('',(#16579,#16580,#16581,#16582,#16583));
#6854=EDGE_LOOP('',(#16584,#16585,#16586,#16587));
#6855=EDGE_LOOP('',(#16588,#16589,#16590,#16591));
#6856=EDGE_LOOP('',(#16592,#16593,#16594,#16595,#16596,#16597,#16598));
#6857=EDGE_LOOP('',(#16599,#16600,#16601,#16602,#16603,#16604));
#6858=EDGE_LOOP('',(#16605,#16606,#16607,#16608,#16609));
#6859=EDGE_LOOP('',(#16610,#16611,#16612,#16613,#16614,#16615,#16616));
#6860=EDGE_LOOP('',(#16617,#16618,#16619,#16620,#16621,#16622));
#6861=EDGE_LOOP('',(#16623));
#6862=EDGE_LOOP('',(#16624,#16625,#16626,#16627,#16628,#16629));
#6863=EDGE_LOOP('',(#16630,#16631,#16632,#16633));
#6864=EDGE_LOOP('',(#16634,#16635,#16636,#16637));
#6865=EDGE_LOOP('',(#16638,#16639,#16640,#16641));
#6866=EDGE_LOOP('',(#16642,#16643,#16644,#16645));
#6867=EDGE_LOOP('',(#16646,#16647,#16648,#16649));
#6868=EDGE_LOOP('',(#16650,#16651,#16652,#16653));
#6869=EDGE_LOOP('',(#16654,#16655,#16656,#16657));
#6870=EDGE_LOOP('',(#16658,#16659,#16660,#16661));
#6871=EDGE_LOOP('',(#16662,#16663,#16664,#16665));
#6872=EDGE_LOOP('',(#16666,#16667,#16668,#16669));
#6873=EDGE_LOOP('',(#16670,#16671,#16672,#16673));
#6874=EDGE_LOOP('',(#16674,#16675,#16676,#16677));
#6875=EDGE_LOOP('',(#16678,#16679,#16680,#16681));
#6876=EDGE_LOOP('',(#16682));
#6877=EDGE_LOOP('',(#16683,#16684,#16685,#16686,#16687,#16688));
#6878=EDGE_LOOP('',(#16689,#16690,#16691,#16692,#16693));
#6879=EDGE_LOOP('',(#16694,#16695,#16696,#16697,#16698,#16699,#16700));
#6880=EDGE_LOOP('',(#16701,#16702));
#6881=EDGE_LOOP('',(#16703,#16704));
#6882=EDGE_LOOP('',(#16705,#16706,#16707));
#6883=EDGE_LOOP('',(#16708,#16709,#16710,#16711,#16712,#16713,#16714,#16715));
#6884=EDGE_LOOP('',(#16716,#16717,#16718,#16719,#16720,#16721));
#6885=EDGE_LOOP('',(#16722,#16723,#16724,#16725));
#6886=EDGE_LOOP('',(#16726,#16727,#16728,#16729,#16730,#16731));
#6887=EDGE_LOOP('',(#16732,#16733,#16734,#16735,#16736,#16737));
#6888=EDGE_LOOP('',(#16738,#16739,#16740,#16741,#16742,#16743,#16744,#16745));
#6889=EDGE_LOOP('',(#16746,#16747));
#6890=EDGE_LOOP('',(#16748,#16749));
#6891=EDGE_LOOP('',(#16750,#16751,#16752,#16753));
#6892=EDGE_LOOP('',(#16754,#16755,#16756,#16757));
#6893=EDGE_LOOP('',(#16758,#16759,#16760,#16761,#16762,#16763,#16764));
#6894=EDGE_LOOP('',(#16765));
#6895=EDGE_LOOP('',(#16766,#16767,#16768,#16769));
#6896=EDGE_LOOP('',(#16770,#16771,#16772,#16773));
#6897=EDGE_LOOP('',(#16774));
#6898=EDGE_LOOP('',(#16775,#16776,#16777,#16778,#16779,#16780));
#6899=EDGE_LOOP('',(#16781,#16782,#16783,#16784,#16785,#16786));
#6900=EDGE_LOOP('',(#16787,#16788,#16789,#16790));
#6901=EDGE_LOOP('',(#16791,#16792,#16793,#16794));
#6902=EDGE_LOOP('',(#16795,#16796,#16797,#16798));
#6903=EDGE_LOOP('',(#16799,#16800,#16801,#16802));
#6904=EDGE_LOOP('',(#16803,#16804,#16805,#16806));
#6905=EDGE_LOOP('',(#16807,#16808,#16809,#16810,#16811,#16812,#16813,#16814,
#16815,#16816,#16817,#16818,#16819,#16820));
#6906=EDGE_LOOP('',(#16821));
#6907=EDGE_LOOP('',(#16822,#16823,#16824,#16825));
#6908=EDGE_LOOP('',(#16826,#16827,#16828,#16829));
#6909=EDGE_LOOP('',(#16830,#16831,#16832,#16833));
#6910=EDGE_LOOP('',(#16834,#16835,#16836,#16837));
#6911=EDGE_LOOP('',(#16838,#16839,#16840,#16841));
#6912=EDGE_LOOP('',(#16842,#16843,#16844,#16845,#16846,#16847));
#6913=EDGE_LOOP('',(#16848,#16849,#16850,#16851));
#6914=EDGE_LOOP('',(#16852,#16853,#16854,#16855,#16856,#16857,#16858,#16859,
#16860,#16861,#16862,#16863));
#6915=EDGE_LOOP('',(#16864,#16865,#16866,#16867));
#6916=EDGE_LOOP('',(#16868,#16869,#16870,#16871));
#6917=EDGE_LOOP('',(#16872,#16873,#16874,#16875,#16876,#16877,#16878,#16879,
#16880,#16881,#16882,#16883,#16884,#16885));
#6918=EDGE_LOOP('',(#16886,#16887,#16888,#16889,#16890,#16891,#16892,#16893,
#16894,#16895));
#6919=EDGE_LOOP('',(#16896,#16897,#16898));
#6920=EDGE_LOOP('',(#16899,#16900,#16901,#16902));
#6921=EDGE_LOOP('',(#16903,#16904,#16905));
#6922=EDGE_LOOP('',(#16906,#16907,#16908,#16909,#16910,#16911));
#6923=EDGE_LOOP('',(#16912,#16913,#16914,#16915,#16916,#16917,#16918,#16919,
#16920,#16921,#16922,#16923));
#6924=EDGE_LOOP('',(#16924,#16925,#16926,#16927,#16928,#16929,#16930));
#6925=EDGE_LOOP('',(#16931,#16932,#16933,#16934,#16935,#16936));
#6926=EDGE_LOOP('',(#16937,#16938,#16939,#16940));
#6927=EDGE_LOOP('',(#16941,#16942,#16943,#16944));
#6928=EDGE_LOOP('',(#16945,#16946,#16947,#16948,#16949,#16950));
#6929=EDGE_LOOP('',(#16951,#16952,#16953,#16954,#16955,#16956));
#6930=EDGE_LOOP('',(#16957));
#6931=EDGE_LOOP('',(#16958,#16959,#16960,#16961));
#6932=EDGE_LOOP('',(#16962,#16963,#16964,#16965));
#6933=EDGE_LOOP('',(#16966,#16967,#16968,#16969));
#6934=EDGE_LOOP('',(#16970,#16971,#16972,#16973));
#6935=EDGE_LOOP('',(#16974,#16975,#16976,#16977,#16978,#16979,#16980));
#6936=EDGE_LOOP('',(#16981,#16982,#16983,#16984));
#6937=EDGE_LOOP('',(#16985,#16986,#16987,#16988));
#6938=EDGE_LOOP('',(#16989));
#6939=EDGE_LOOP('',(#16990,#16991,#16992,#16993));
#6940=EDGE_LOOP('',(#16994,#16995,#16996,#16997));
#6941=EDGE_LOOP('',(#16998,#16999,#17000,#17001));
#6942=EDGE_LOOP('',(#17002,#17003,#17004,#17005));
#6943=EDGE_LOOP('',(#17006));
#6944=EDGE_LOOP('',(#17007,#17008,#17009,#17010));
#6945=EDGE_LOOP('',(#17011,#17012,#17013,#17014));
#6946=EDGE_LOOP('',(#17015,#17016,#17017,#17018));
#6947=EDGE_LOOP('',(#17019,#17020,#17021,#17022));
#6948=EDGE_LOOP('',(#17023,#17024,#17025,#17026,#17027,#17028));
#6949=EDGE_LOOP('',(#17029));
#6950=EDGE_LOOP('',(#17030,#17031,#17032,#17033));
#6951=EDGE_LOOP('',(#17034,#17035,#17036,#17037));
#6952=EDGE_LOOP('',(#17038,#17039,#17040,#17041,#17042,#17043,#17044,#17045,
#17046,#17047,#17048,#17049,#17050,#17051,#17052,#17053,#17054,#17055,#17056,
#17057,#17058,#17059));
#6953=EDGE_LOOP('',(#17060));
#6954=EDGE_LOOP('',(#17061,#17062,#17063,#17064,#17065,#17066,#17067));
#6955=EDGE_LOOP('',(#17068,#17069,#17070,#17071));
#6956=EDGE_LOOP('',(#17072,#17073,#17074,#17075,#17076,#17077));
#6957=EDGE_LOOP('',(#17078,#17079,#17080,#17081,#17082,#17083,#17084,#17085,
#17086,#17087));
#6958=EDGE_LOOP('',(#17088,#17089,#17090,#17091,#17092,#17093));
#6959=EDGE_LOOP('',(#17094,#17095,#17096,#17097,#17098));
#6960=EDGE_LOOP('',(#17099,#17100,#17101,#17102));
#6961=EDGE_LOOP('',(#17103,#17104,#17105,#17106,#17107));
#6962=EDGE_LOOP('',(#17108,#17109,#17110,#17111,#17112,#17113));
#6963=EDGE_LOOP('',(#17114,#17115,#17116,#17117,#17118,#17119,#17120,#17121));
#6964=EDGE_LOOP('',(#17122,#17123,#17124,#17125,#17126,#17127));
#6965=EDGE_LOOP('',(#17128,#17129,#17130,#17131));
#6966=EDGE_LOOP('',(#17132,#17133,#17134,#17135,#17136,#17137,#17138,#17139,
#17140,#17141,#17142,#17143));
#6967=EDGE_LOOP('',(#17144));
#6968=EDGE_LOOP('',(#17145));
#6969=EDGE_LOOP('',(#17146));
#6970=EDGE_LOOP('',(#17147));
#6971=EDGE_LOOP('',(#17148,#17149,#17150,#17151,#17152));
#6972=EDGE_LOOP('',(#17153,#17154,#17155,#17156,#17157,#17158,#17159,#17160,
#17161));
#6973=EDGE_LOOP('',(#17162,#17163,#17164,#17165));
#6974=EDGE_LOOP('',(#17166,#17167,#17168,#17169,#17170));
#6975=EDGE_LOOP('',(#17171));
#6976=EDGE_LOOP('',(#17172));
#6977=EDGE_LOOP('',(#17173));
#6978=EDGE_LOOP('',(#17174,#17175,#17176));
#6979=EDGE_LOOP('',(#17177,#17178,#17179));
#6980=EDGE_LOOP('',(#17180,#17181,#17182));
#6981=EDGE_LOOP('',(#17183,#17184,#17185));
#6982=EDGE_LOOP('',(#17186,#17187,#17188));
#6983=EDGE_LOOP('',(#17189,#17190,#17191));
#6984=EDGE_LOOP('',(#17192,#17193,#17194,#17195,#17196,#17197));
#6985=EDGE_LOOP('',(#17198,#17199,#17200));
#6986=EDGE_LOOP('',(#17201,#17202,#17203));
#6987=EDGE_LOOP('',(#17204,#17205,#17206));
#6988=EDGE_LOOP('',(#17207,#17208,#17209));
#6989=EDGE_LOOP('',(#17210,#17211,#17212));
#6990=EDGE_LOOP('',(#17213,#17214,#17215));
#6991=EDGE_LOOP('',(#17216,#17217,#17218,#17219,#17220,#17221));
#6992=EDGE_LOOP('',(#17222,#17223,#17224,#17225,#17226,#17227));
#6993=EDGE_LOOP('',(#17228,#17229,#17230,#17231,#17232,#17233));
#6994=EDGE_LOOP('',(#17234,#17235,#17236,#17237,#17238,#17239));
#6995=EDGE_LOOP('',(#17240,#17241,#17242,#17243,#17244,#17245));
#6996=EDGE_LOOP('',(#17246,#17247,#17248,#17249,#17250,#17251));
#6997=CIRCLE('',#18352,30.);
#6998=CIRCLE('',#18353,5.);
#6999=CIRCLE('',#18354,25.);
#7000=CIRCLE('',#18356,250.);
#7001=CIRCLE('',#18357,250.);
#7002=CIRCLE('',#18358,5.);
#7003=CIRCLE('',#18359,245.);
#7004=CIRCLE('',#18361,35.);
#7005=CIRCLE('',#18363,35.);
#7006=CIRCLE('',#18365,35.);
#7007=CIRCLE('',#18367,35.);
#7008=CIRCLE('',#18369,35.);
#7009=CIRCLE('',#18370,35.);
#7010=CIRCLE('',#18371,35.);
#7011=CIRCLE('',#18373,35.);
#7012=CIRCLE('',#18375,35.);
#7013=CIRCLE('',#18377,35.);
#7014=CIRCLE('',#18379,35.);
#7015=CIRCLE('',#18382,2.5);
#7016=CIRCLE('',#18383,2.5);
#7017=CIRCLE('',#18385,2.49999999999997);
#7018=CIRCLE('',#18386,2.49999999999997);
#7019=CIRCLE('',#18388,2.5);
#7020=CIRCLE('',#18389,2.5);
#7021=CIRCLE('',#18391,2.5);
#7022=CIRCLE('',#18392,2.5);
#7023=CIRCLE('',#18394,2.49999999999997);
#7024=CIRCLE('',#18395,2.49999999999997);
#7025=CIRCLE('',#18397,2.5);
#7026=CIRCLE('',#18398,2.5);
#7027=CIRCLE('',#18400,2.5);
#7028=CIRCLE('',#18401,2.5);
#7029=CIRCLE('',#18403,2.5);
#7030=CIRCLE('',#18404,2.5);
#7031=CIRCLE('',#18406,19.);
#7032=CIRCLE('',#18408,19.);
#7033=CIRCLE('',#18410,15.);
#7034=CIRCLE('',#18412,15.);
#7035=CIRCLE('',#18414,25.);
#7036=CIRCLE('',#18416,2.5);
#7037=CIRCLE('',#18417,2.5);
#7038=CIRCLE('',#18419,2.5);
#7039=CIRCLE('',#18420,2.5);
#7040=CIRCLE('',#18422,2.5);
#7041=CIRCLE('',#18423,2.5);
#7042=CIRCLE('',#18425,2.5);
#7043=CIRCLE('',#18426,2.5);
#7044=CIRCLE('',#18428,2.5);
#7045=CIRCLE('',#18429,2.5);
#7046=CIRCLE('',#18431,2.5);
#7047=CIRCLE('',#18432,2.5);
#7048=CIRCLE('',#18434,2.5);
#7049=CIRCLE('',#18435,2.5);
#7050=CIRCLE('',#18437,2.5);
#7051=CIRCLE('',#18438,2.5);
#7052=CIRCLE('',#18440,2.50000000000001);
#7053=CIRCLE('',#18441,2.50000000000001);
#7054=CIRCLE('',#18443,2.5);
#7055=CIRCLE('',#18444,2.5);
#7056=CIRCLE('',#18446,2.5);
#7057=CIRCLE('',#18447,2.5);
#7058=CIRCLE('',#18449,2.5);
#7059=CIRCLE('',#18450,2.5);
#7060=CIRCLE('',#18452,2.5);
#7061=CIRCLE('',#18453,2.5);
#7062=CIRCLE('',#18455,2.5);
#7063=CIRCLE('',#18456,2.5);
#7064=CIRCLE('',#18458,2.5);
#7065=CIRCLE('',#18459,2.5);
#7066=CIRCLE('',#18461,250.);
#7067=CIRCLE('',#18463,275.);
#7068=CIRCLE('',#18464,275.);
#7069=CIRCLE('',#18466,240.);
#7070=CIRCLE('',#18467,240.);
#7071=CIRCLE('',#18473,5.);
#7072=CIRCLE('',#18474,5.);
#7073=CIRCLE('',#18475,5.00000000000003);
#7074=CIRCLE('',#18476,5.);
#7075=CIRCLE('',#18478,5.);
#7076=CIRCLE('',#18479,5.);
#7077=CIRCLE('',#18480,5.00000000000003);
#7078=CIRCLE('',#18481,5.);
#7079=CIRCLE('',#18491,5.);
#7080=CIRCLE('',#18492,5.);
#7081=CIRCLE('',#18493,5.);
#7082=CIRCLE('',#18494,5.00000000000003);
#7083=CIRCLE('',#18496,5.);
#7084=CIRCLE('',#18497,5.00000000000003);
#7085=CIRCLE('',#18498,5.);
#7086=CIRCLE('',#18499,5.);
#7087=CIRCLE('',#18538,206.);
#7088=CIRCLE('',#18539,206.);
#7089=CIRCLE('',#18541,145.404667636179);
#7090=CIRCLE('',#18542,145.404667636179);
#7091=CIRCLE('',#18544,5.);
#7092=CIRCLE('',#18546,147.404667636179);
#7093=CIRCLE('',#18547,147.404667636179);
#7094=CIRCLE('',#18549,204.);
#7095=CIRCLE('',#18551,204.);
#7096=CIRCLE('',#18552,145.404667636179);
#7097=CIRCLE('',#18553,206.);
#7098=CIRCLE('',#18556,145.404667636179);
#7099=CIRCLE('',#18558,206.);
#7100=CIRCLE('',#18570,206.);
#7101=CIRCLE('',#18571,206.);
#7102=CIRCLE('',#18573,145.404667636179);
#7103=CIRCLE('',#18574,145.404667636179);
#7104=CIRCLE('',#18576,5.);
#7105=CIRCLE('',#18578,147.404667636179);
#7106=CIRCLE('',#18579,147.404667636179);
#7107=CIRCLE('',#18581,204.);
#7108=CIRCLE('',#18582,204.);
#7109=CIRCLE('',#18584,204.);
#7110=CIRCLE('',#18585,204.);
#7111=CIRCLE('',#18586,145.404667636179);
#7112=CIRCLE('',#18587,206.);
#7113=CIRCLE('',#18590,145.404667636179);
#7114=CIRCLE('',#18592,206.);
#7115=CIRCLE('',#18604,10.);
#7116=CIRCLE('',#18605,10.);
#7117=CIRCLE('',#18607,10.);
#7118=CIRCLE('',#18608,10.);
#7119=CIRCLE('',#18610,27.9488084273619);
#7120=CIRCLE('',#18611,27.9488084273619);
#7121=CIRCLE('',#18613,17.4625);
#7122=CIRCLE('',#18614,17.4625);
#7123=CIRCLE('',#18616,25.);
#7124=CIRCLE('',#18617,25.);
#7125=CIRCLE('',#18619,204.);
#7126=CIRCLE('',#18620,204.);
#7127=CIRCLE('',#18622,200.);
#7128=CIRCLE('',#18623,200.);
#7129=CIRCLE('',#18624,200.);
#7130=CIRCLE('',#18625,200.);
#7131=CIRCLE('',#18626,200.);
#7132=CIRCLE('',#18627,200.);
#7133=CIRCLE('',#18628,200.);
#7134=CIRCLE('',#18629,200.);
#7135=CIRCLE('',#18630,200.);
#7136=CIRCLE('',#18631,200.);
#7137=CIRCLE('',#18633,10.);
#7138=CIRCLE('',#18634,122.05461305459);
#7139=CIRCLE('',#18635,77.4625);
#7140=CIRCLE('',#18636,122.05461305459);
#7141=CIRCLE('',#18637,27.9488084273619);
#7142=CIRCLE('',#18638,122.05461305459);
#7143=CIRCLE('',#18639,77.4625);
#7144=CIRCLE('',#18640,122.05461305459);
#7145=CIRCLE('',#18641,10.);
#7146=CIRCLE('',#18642,25.);
#7147=CIRCLE('',#18643,25.);
#7148=CIRCLE('',#18644,25.);
#7149=CIRCLE('',#18645,25.);
#7150=CIRCLE('',#18646,25.);
#7151=CIRCLE('',#18647,25.);
#7152=CIRCLE('',#18648,25.);
#7153=CIRCLE('',#18649,25.);
#7154=CIRCLE('',#18651,25.);
#7155=CIRCLE('',#18653,25.);
#7156=CIRCLE('',#18655,25.);
#7157=CIRCLE('',#18657,25.);
#7158=CIRCLE('',#18659,25.);
#7159=CIRCLE('',#18661,25.);
#7160=CIRCLE('',#18663,25.);
#7161=CIRCLE('',#18665,25.);
#7162=CIRCLE('',#18669,122.05461305459);
#7163=CIRCLE('',#18671,77.4625);
#7164=CIRCLE('',#18673,122.05461305459);
#7165=CIRCLE('',#18675,122.05461305459);
#7166=CIRCLE('',#18677,77.4625);
#7167=CIRCLE('',#18679,122.05461305459);
#7168=CIRCLE('',#18681,10.);
#7169=CIRCLE('',#18682,27.9488084273619);
#7170=CIRCLE('',#18683,10.);
#7171=CIRCLE('',#18723,14.);
#7172=CIRCLE('',#18724,208.);
#7173=CIRCLE('',#18725,208.);
#7174=CIRCLE('',#18726,14.);
#7175=CIRCLE('',#18727,14.);
#7176=CIRCLE('',#18728,14.);
#7177=CIRCLE('',#18730,15.);
#7178=CIRCLE('',#18731,15.);
#7179=CIRCLE('',#18732,207.);
#7180=CIRCLE('',#18733,207.);
#7181=CIRCLE('',#18734,15.);
#7182=CIRCLE('',#18735,15.);
#7183=CIRCLE('',#18736,3.99999999999999);
#7184=CIRCLE('',#18737,3.99999999999999);
#7185=CIRCLE('',#18739,14.);
#7186=CIRCLE('',#18741,14.);
#7187=CIRCLE('',#18742,5.);
#7188=CIRCLE('',#18743,5.00000000000001);
#7189=CIRCLE('',#18745,15.);
#7190=CIRCLE('',#18747,15.);
#7191=CIRCLE('',#18754,6.75000000000001);
#7192=CIRCLE('',#18755,6.75000000000001);
#7193=CIRCLE('',#18757,6.74999999999998);
#7194=CIRCLE('',#18758,6.74999999999998);
#7195=CIRCLE('',#18760,6.74999999999998);
#7196=CIRCLE('',#18761,6.74999999999998);
#7197=CIRCLE('',#18763,6.75000000000001);
#7198=CIRCLE('',#18764,6.75000000000001);
#7199=CIRCLE('',#18795,96.161193339026);
#7200=CIRCLE('',#18796,96.161193339026);
#7201=CIRCLE('',#18798,2.5);
#7202=CIRCLE('',#18799,2.5);
#7203=CIRCLE('',#18801,2.5);
#7204=CIRCLE('',#18802,2.5);
#7205=CIRCLE('',#18804,2.5);
#7206=CIRCLE('',#18805,2.5);
#7207=CIRCLE('',#18807,2.5);
#7208=CIRCLE('',#18808,2.5);
#7209=CIRCLE('',#18810,2.5);
#7210=CIRCLE('',#18811,2.5);
#7211=CIRCLE('',#18813,2.5);
#7212=CIRCLE('',#18814,2.5);
#7213=CIRCLE('',#18816,2.5);
#7214=CIRCLE('',#18817,2.5);
#7215=CIRCLE('',#18819,2.5);
#7216=CIRCLE('',#18820,2.5);
#7217=CIRCLE('',#18822,2.50000000000001);
#7218=CIRCLE('',#18823,2.50000000000001);
#7219=CIRCLE('',#18825,2.5);
#7220=CIRCLE('',#18826,2.5);
#7221=CIRCLE('',#18828,2.5);
#7222=CIRCLE('',#18829,2.5);
#7223=CIRCLE('',#18831,2.5);
#7224=CIRCLE('',#18832,2.5);
#7225=CIRCLE('',#18834,2.5);
#7226=CIRCLE('',#18835,2.5);
#7227=CIRCLE('',#18837,2.5);
#7228=CIRCLE('',#18838,2.5);
#7229=CIRCLE('',#18840,2.5);
#7230=CIRCLE('',#18841,2.5);
#7231=CIRCLE('',#18843,275.);
#7232=CIRCLE('',#18844,275.);
#7233=CIRCLE('',#18848,96.161193339026);
#7234=CIRCLE('',#18849,96.161193339026);
#7235=CIRCLE('',#18854,25.3339394440353);
#7236=CIRCLE('',#18855,5.00000000000101);
#7237=CIRCLE('',#18856,27.3317482398799);
#7238=CIRCLE('',#18857,27.3317482398799);
#7239=CIRCLE('',#18859,28.6682517601201);
#7240=CIRCLE('',#18860,4.99999999999874);
#7241=CIRCLE('',#18861,29.7575436501051);
#7242=CIRCLE('',#18862,29.7575436501051);
#7243=CIRCLE('',#18863,28.6682517601201);
#7244=CIRCLE('',#18865,45.3097394023382);
#7245=CIRCLE('',#18866,4.00000000000009);
#7246=CIRCLE('',#18867,49.0555555555557);
#7247=CIRCLE('',#18868,49.0555555555557);
#7248=CIRCLE('',#18869,45.3097394023382);
#7249=CIRCLE('',#18871,32.793965079916);
#7250=CIRCLE('',#18872,3.99999999999933);
#7251=CIRCLE('',#18873,34.8097394023382);
#7252=CIRCLE('',#18874,34.8097394023382);
#7253=CIRCLE('',#18875,32.793965079916);
#7254=CIRCLE('',#18877,55.);
#7255=CIRCLE('',#18878,55.);
#7256=CIRCLE('',#18881,50.0000000000001);
#7257=CIRCLE('',#18887,0.857142857149273);
#7258=CIRCLE('',#18888,0.857142857149273);
#7259=CIRCLE('',#18889,0.800000000003749);
#7260=CIRCLE('',#18891,0.999999999962782);
#7261=CIRCLE('',#18894,0.499999999966139);
#7262=CIRCLE('',#18906,9.75000000013422);
#7263=CIRCLE('',#18907,19.9999999999997);
#7264=CIRCLE('',#18908,6.75000000007079);
#7265=CIRCLE('',#18909,6.75000000007079);
#7266=CIRCLE('',#18911,6.75000000000001);
#7267=CIRCLE('',#18912,6.75000000000001);
#7268=CIRCLE('',#18914,6.75);
#7269=CIRCLE('',#18915,6.75);
#7270=CIRCLE('',#18917,6.75000000000001);
#7271=CIRCLE('',#18918,6.75000000000001);
#7272=CIRCLE('',#18920,6.75);
#7273=CIRCLE('',#18921,6.75);
#7274=CIRCLE('',#18923,7.00000000000001);
#7275=CIRCLE('',#18925,7.00000000000001);
#7276=CIRCLE('',#18928,27.5);
#7277=CIRCLE('',#18929,27.5);
#7278=CIRCLE('',#18931,100.);
#7279=CIRCLE('',#18932,105.377972911614);
#7280=CIRCLE('',#18933,107.1412427187);
#7281=CIRCLE('',#18934,106.259607815157);
#7282=CIRCLE('',#18936,22.);
#7283=CIRCLE('',#18937,22.);
#7284=CIRCLE('',#18939,7.);
#7285=CIRCLE('',#18940,7.);
#7286=CIRCLE('',#18942,7.);
#7287=CIRCLE('',#18943,7.);
#7288=CIRCLE('',#18944,7.);
#7289=CIRCLE('',#18945,7.);
#7290=CIRCLE('',#18947,7.);
#7291=CIRCLE('',#18949,7.);
#7292=CIRCLE('',#18950,7.);
#7293=CIRCLE('',#18951,7.);
#7294=CIRCLE('',#18954,80.);
#7295=CIRCLE('',#18955,80.);
#7296=CIRCLE('',#18957,40.);
#7297=CIRCLE('',#18958,40.);
#7298=CIRCLE('',#18965,12.);
#7299=CIRCLE('',#18968,53.);
#7300=CIRCLE('',#18969,53.);
#7301=CIRCLE('',#18970,53.);
#7302=CIRCLE('',#18972,4.5);
#7303=CIRCLE('',#18973,4.5);
#7304=CIRCLE('',#18975,4.5);
#7305=CIRCLE('',#18976,4.5);
#7306=CIRCLE('',#18978,4.5);
#7307=CIRCLE('',#18979,4.5);
#7308=CIRCLE('',#18981,4.5);
#7309=CIRCLE('',#18982,4.5);
#7310=CIRCLE('',#18984,20.);
#7311=CIRCLE('',#18985,20.);
#7312=CIRCLE('',#18987,12.);
#7313=CIRCLE('',#18989,10.);
#7314=CIRCLE('',#18994,68.);
#7315=CIRCLE('',#18995,76.5);
#7316=CIRCLE('',#18996,68.);
#7317=CIRCLE('',#18997,76.5);
#7318=CIRCLE('',#18998,68.);
#7319=CIRCLE('',#18999,68.);
#7320=CIRCLE('',#19000,76.5);
#7321=CIRCLE('',#19001,68.);
#7322=CIRCLE('',#19002,76.5);
#7323=CIRCLE('',#19005,7.);
#7324=CIRCLE('',#19006,7.00000000000001);
#7325=CIRCLE('',#19007,7.00000000000001);
#7326=CIRCLE('',#19008,7.);
#7327=CIRCLE('',#19010,12.);
#7328=CIRCLE('',#19011,12.);
#7329=CIRCLE('',#19013,68.);
#7330=CIRCLE('',#19014,68.);
#7331=CIRCLE('',#19015,68.);
#7332=CIRCLE('',#19017,6.0000000000113);
#7333=CIRCLE('',#19019,4.);
#7334=CIRCLE('',#19020,4.);
#7335=CIRCLE('',#19022,4.);
#7336=CIRCLE('',#19023,4.);
#7337=CIRCLE('',#19025,4.);
#7338=CIRCLE('',#19026,4.);
#7339=CIRCLE('',#19028,4.);
#7340=CIRCLE('',#19029,4.);
#7341=CIRCLE('',#19031,17.4625);
#7342=CIRCLE('',#19032,17.4625);
#7343=CIRCLE('',#19033,17.4625);
#7344=CIRCLE('',#19034,17.4625);
#7345=CIRCLE('',#19035,17.4625);
#7346=CIRCLE('',#19036,17.4625);
#7347=CIRCLE('',#19038,8.00000000000001);
#7348=CIRCLE('',#19039,7.99999999999999);
#7349=CIRCLE('',#19041,8.00000000000001);
#7350=CIRCLE('',#19042,8.00000000000001);
#7351=CIRCLE('',#19044,16.4625);
#7352=CIRCLE('',#19046,7.00000000000001);
#7353=CIRCLE('',#19047,7.00000000000001);
#7354=CIRCLE('',#19049,7.00000000000001);
#7355=CIRCLE('',#19050,7.00000000000001);
#7356=CIRCLE('',#19052,3.);
#7357=CIRCLE('',#19053,3.);
#7358=CIRCLE('',#19055,3.00000000000307);
#7359=CIRCLE('',#19056,3.00000000000307);
#7360=CIRCLE('',#19058,3.0000000000021);
#7361=CIRCLE('',#19059,3.0000000000021);
#7362=CIRCLE('',#19061,2.99999999999927);
#7363=CIRCLE('',#19062,2.99999999999927);
#7364=CIRCLE('',#19064,68.);
#7365=CIRCLE('',#19065,68.);
#7366=CIRCLE('',#19067,6.7500000000354);
#7367=CIRCLE('',#19068,6.7500000000354);
#7368=CIRCLE('',#19070,944.519985714474);
#7369=CIRCLE('',#19071,945.);
#7370=CIRCLE('',#19073,5.49999999998363);
#7371=CIRCLE('',#19074,5.49999999998363);
#7372=CIRCLE('',#19076,5.5);
#7373=CIRCLE('',#19077,5.5);
#7374=CIRCLE('',#19079,941.808101337222);
#7375=CIRCLE('',#19080,941.808086415458);
#7376=CIRCLE('',#19081,942.);
#7377=CIRCLE('',#19082,941.808086538241);
#7378=CIRCLE('',#19083,941.808101200289);
#7379=CIRCLE('',#19085,8.8000000000042);
#7380=CIRCLE('',#19086,8.80000000000425);
#7381=CIRCLE('',#19088,8.80000000000415);
#7382=CIRCLE('',#19089,8.80000000000425);
#7383=CIRCLE('',#19091,6.34999999994079);
#7384=CIRCLE('',#19093,5.5);
#7385=CIRCLE('',#19094,5.5);
#7386=CIRCLE('',#19095,5.5);
#7387=CIRCLE('',#19097,179.500000000001);
#7388=CIRCLE('',#19098,179.500000000005);
#7389=CIRCLE('',#19111,16.);
#7390=CIRCLE('',#19112,16.0000000000001);
#7391=CIRCLE('',#19113,179.500000000005);
#7392=CIRCLE('',#19114,15.9999999999999);
#7393=CIRCLE('',#19115,16.);
#7394=CIRCLE('',#19116,16.);
#7395=CIRCLE('',#19117,15.9999999999999);
#7396=CIRCLE('',#19118,179.500000000006);
#7397=CIRCLE('',#19119,16.);
#7398=CIRCLE('',#19120,15.9999999999999);
#7399=CIRCLE('',#19121,179.5);
#7400=CIRCLE('',#19131,7.00000000000003);
#7401=CIRCLE('',#19133,7.00000000000011);
#7402=CIRCLE('',#19134,7.00000000000007);
#7403=CIRCLE('',#19136,7.00000000000003);
#7404=CIRCLE('',#19144,7.00000000000001);
#7405=CIRCLE('',#19146,7.00000000000006);
#7406=CIRCLE('',#19147,7.00000000000003);
#7407=CIRCLE('',#19149,7.00000000000006);
#7408=CIRCLE('',#19157,7.00000000000001);
#7409=CIRCLE('',#19159,6.99999999999996);
#7410=CIRCLE('',#19160,6.99999999999999);
#7411=CIRCLE('',#19162,7.00000000000001);
#7412=CIRCLE('',#19164,7.00000000000001);
#7413=CIRCLE('',#19172,6.99999999999999);
#7414=CIRCLE('',#19174,6.99999999999999);
#7415=CIRCLE('',#19176,7.00000000000001);
#7416=CIRCLE('',#19178,16.0000000000001);
#7417=CIRCLE('',#19181,15.9999999999999);
#7418=CIRCLE('',#19183,179.500000000001);
#7419=CIRCLE('',#19185,16.0000000000001);
#7420=CIRCLE('',#19188,15.9999999999999);
#7421=CIRCLE('',#19190,179.500000000007);
#7422=CIRCLE('',#19192,16.);
#7423=CIRCLE('',#19195,15.9999999999999);
#7424=CIRCLE('',#19197,16.);
#7425=CIRCLE('',#19200,15.9999999999999);
#7426=CIRCLE('',#19202,179.500000000005);
#7427=CIRCLE('',#19204,19.7365042497449);
#7428=CIRCLE('',#19206,19.7365042497449);
#7429=CIRCLE('',#19208,19.7365042498482);
#7430=CIRCLE('',#19210,19.7365042497453);
#7431=CIRCLE('',#19212,19.7365042497445);
#7432=CIRCLE('',#19214,19.7365042497295);
#7433=CIRCLE('',#19216,19.7365042497448);
#7434=CIRCLE('',#19218,19.7365042497449);
#7435=CIRCLE('',#19220,19.7365042497272);
#7436=CIRCLE('',#19222,19.736504249745);
#7437=CIRCLE('',#19224,19.7365042497451);
#7438=CIRCLE('',#19226,19.7365042497215);
#7439=CIRCLE('',#19230,6.99999999999999);
#7440=CIRCLE('',#19233,7.00000000000003);
#7441=CIRCLE('',#19235,6.99999999999996);
#7442=CIRCLE('',#19238,6.99999999999997);
#7443=CIRCLE('',#19241,80.4999999999992);
#7444=CIRCLE('',#19245,80.4999999999997);
#7445=CIRCLE('',#19249,80.4999999999963);
#7446=CIRCLE('',#19253,80.4999999999957);
#7447=CIRCLE('',#19256,150.000000000136);
#7448=CIRCLE('',#19257,149.99999999991);
#7449=CIRCLE('',#19258,150.000000000245);
#7450=CIRCLE('',#19259,149.999999999925);
#7451=CIRCLE('',#19260,150.000000000098);
#7452=CIRCLE('',#19261,150.000000000117);
#7453=CIRCLE('',#19262,150.000000000073);
#7454=CIRCLE('',#19267,6.99999999999999);
#7455=CIRCLE('',#19270,7.00000000000003);
#7456=CIRCLE('',#19273,7.00000000000001);
#7457=CIRCLE('',#19276,6.99999999999999);
#7458=CIRCLE('',#19279,941.808101449981);
#7459=CIRCLE('',#19281,941.808118804699);
#7460=CIRCLE('',#19283,941.808118685871);
#7461=CIRCLE('',#19285,941.808101328173);
#7462=CIRCLE('',#19287,219.614732166431);
#7463=CIRCLE('',#19293,199.807995098081);
#7464=CIRCLE('',#19295,199.807995098081);
#7465=CIRCLE('',#19297,199.807995098081);
#7466=CIRCLE('',#19299,199.807995098081);
#7467=CIRCLE('',#19300,22.0736331396068);
#7468=CIRCLE('',#19302,941.807993346891);
#7469=CIRCLE('',#19304,941.807993346891);
#7470=CIRCLE('',#19305,15.0039593060322);
#7471=CIRCLE('',#19307,941.807993346891);
#7472=CIRCLE('',#19309,941.807993346891);
#7473=CIRCLE('',#19311,4.);
#7474=CIRCLE('',#19312,4.);
#7475=CIRCLE('',#19313,4.);
#7476=CIRCLE('',#19314,4.);
#7477=CIRCLE('',#19316,22.3000008196592);
#7478=CIRCLE('',#19318,86.00000081803);
#7479=CIRCLE('',#19320,22.3000010500621);
#7480=CIRCLE('',#19322,942.000001054498);
#7481=CIRCLE('',#19324,22.3000013536827);
#7482=CIRCLE('',#19326,86.0000013640202);
#7483=CIRCLE('',#19328,22.3000017511903);
#7484=CIRCLE('',#19330,22.3000017511903);
#7485=CIRCLE('',#19332,86.0000013640202);
#7486=CIRCLE('',#19334,32.8000013531573);
#7487=CIRCLE('',#19336,200.000000812291);
#7488=CIRCLE('',#19338,32.8000008122913);
#7489=CIRCLE('',#19340,86.0000008122913);
#7490=CIRCLE('',#19342,22.3000008122913);
#7491=CIRCLE('',#19344,941.999999061101);
#7492=CIRCLE('',#19348,4.);
#7493=CIRCLE('',#19351,4.);
#7494=CIRCLE('',#19353,4.);
#7495=CIRCLE('',#19355,4.);
#7496=CIRCLE('',#19357,14.8404677219111);
#7497=CIRCLE('',#19359,14.840467735277);
#7498=CIRCLE('',#19360,14.8404675855456);
#7499=CIRCLE('',#19362,14.8404677463308);
#7500=CIRCLE('',#19363,14.8409372248161);
#7501=CIRCLE('',#19366,13.3716191641864);
#7502=CIRCLE('',#19368,13.3716183569085);
#7503=CIRCLE('',#19370,14.8404675936254);
#7504=CIRCLE('',#19372,24.7856889787886);
#7505=CIRCLE('',#19373,24.7856889787948);
#7506=CIRCLE('',#19374,944.519985714474);
#7507=CIRCLE('',#19375,24.7856889787948);
#7508=CIRCLE('',#19376,24.7856889787949);
#7509=CIRCLE('',#19377,944.519985714474);
#7510=CIRCLE('',#19378,24.7856889787946);
#7511=CIRCLE('',#19379,34.5199857136054);
#7512=CIRCLE('',#19380,179.519985714474);
#7513=CIRCLE('',#19381,34.5199857136052);
#7514=CIRCLE('',#19382,24.7856889787945);
#7515=CIRCLE('',#19390,25.2657032643209);
#7516=CIRCLE('',#19395,25.2657032643207);
#7517=CIRCLE('',#19397,945.);
#7518=CIRCLE('',#19399,25.2657032643207);
#7519=CIRCLE('',#19404,25.2657032643145);
#7520=CIRCLE('',#19406,25.2657032643204);
#7521=CIRCLE('',#19411,34.9999999991313);
#7522=CIRCLE('',#19413,180.);
#7523=CIRCLE('',#19415,34.9999999991315);
#7524=CIRCLE('',#19420,25.2657032643206);
#7525=CIRCLE('',#19422,945.);
#7526=CIRCLE('',#19436,68.);
#7527=CIRCLE('',#19437,68.);
#7528=CIRCLE('',#19439,77.);
#7529=CIRCLE('',#19440,77.);
#7530=CIRCLE('',#19443,68.);
#7531=CIRCLE('',#19445,68.);
#7532=CIRCLE('',#19447,77.);
#7533=CIRCLE('',#19448,77.);
#7534=CIRCLE('',#19450,68.);
#7535=CIRCLE('',#19451,68.);
#7536=CIRCLE('',#19453,77.);
#7537=CIRCLE('',#19454,77.);
#7538=CIRCLE('',#19456,77.);
#7539=CIRCLE('',#19458,77.);
#7540=CIRCLE('',#19464,4.);
#7541=CIRCLE('',#19465,4.);
#7542=CIRCLE('',#19467,5.);
#7543=CIRCLE('',#19468,5.);
#7544=CIRCLE('',#19472,4.);
#7545=CIRCLE('',#19478,4.);
#7546=CIRCLE('',#19480,5.);
#7547=CIRCLE('',#19481,5.);
#7548=CIRCLE('',#19486,4.);
#7549=CIRCLE('',#19487,4.);
#7550=CIRCLE('',#19489,5.);
#7551=CIRCLE('',#19490,5.);
#7552=CIRCLE('',#19494,5.);
#7553=CIRCLE('',#19495,5.);
#7554=CIRCLE('',#19499,4.);
#7555=CIRCLE('',#19500,4.);
#7556=CIRCLE('',#19505,77.);
#7557=CIRCLE('',#19507,77.);
#7558=CIRCLE('',#19510,4.);
#7559=CIRCLE('',#19515,4.);
#7560=CIRCLE('',#19518,77.);
#7561=CIRCLE('',#19520,77.);
#7562=CIRCLE('',#19523,4.);
#7563=CIRCLE('',#19528,4.);
#7564=CIRCLE('',#19531,77.);
#7565=CIRCLE('',#19533,77.);
#7566=CIRCLE('',#19536,4.);
#7567=CIRCLE('',#19541,4.);
#7568=CIRCLE('',#19544,77.);
#7569=CIRCLE('',#19546,77.);
#7570=CIRCLE('',#19549,4.);
#7571=CIRCLE('',#19554,4.);
#7572=CIRCLE('',#19574,76.5);
#7573=CIRCLE('',#19575,68.);
#7574=CIRCLE('',#19576,68.);
#7575=CIRCLE('',#19579,68.);
#7576=CIRCLE('',#19582,76.5);
#7577=CIRCLE('',#19583,68.);
#7578=CIRCLE('',#19588,68.);
#7579=CIRCLE('',#19589,76.5);
#7580=CIRCLE('',#19592,68.);
#7581=CIRCLE('',#19595,68.);
#7582=CIRCLE('',#19596,76.5);
#7583=CIRCLE('',#19597,68.);
#7584=CIRCLE('',#19600,68.);
#7585=CIRCLE('',#19620,12.);
#7586=CIRCLE('',#19621,12.);
#7587=CIRCLE('',#19623,12.);
#7588=CIRCLE('',#19624,12.);
#7589=CIRCLE('',#19635,10.);
#7590=CIRCLE('',#19637,12.);
#7591=CIRCLE('',#19638,12.);
#7592=CIRCLE('',#19646,4.5);
#7593=CIRCLE('',#19652,12.);
#7594=CIRCLE('',#19655,12.);
#7595=CIRCLE('',#19657,12.);
#7596=CIRCLE('',#19660,12.);
#7597=CIRCLE('',#19662,12.);
#7598=CIRCLE('',#19663,12.);
#7599=CIRCLE('',#19665,12.);
#7600=CIRCLE('',#19668,12.);
#7601=CIRCLE('',#19670,12.);
#7602=CIRCLE('',#19673,12.);
#7603=CIRCLE('',#19683,2.);
#7604=CIRCLE('',#19685,2.);
#7605=CIRCLE('',#19705,6.);
#7606=CIRCLE('',#19707,10.);
#7607=CIRCLE('',#19708,10.);
#7608=CIRCLE('',#19710,2.5);
#7609=CIRCLE('',#19718,10.);
#7610=CIRCLE('',#19719,10.);
#7611=CIRCLE('',#19721,2.5);
#7612=CIRCLE('',#19735,2.);
#7613=CIRCLE('',#19737,2.);
#7614=CIRCLE('',#19746,6.00000000000001);
#7615=CIRCLE('',#19748,10.);
#7616=CIRCLE('',#19749,10.);
#7617=CIRCLE('',#19751,6.);
#7618=CIRCLE('',#19753,10.);
#7619=CIRCLE('',#19755,2.5);
#7620=CIRCLE('',#19765,6.00000000000001);
#7621=CIRCLE('',#19767,10.);
#7622=CIRCLE('',#19769,2.5);
#7623=CIRCLE('',#19796,12.);
#7624=CIRCLE('',#19800,12.);
#7625=CIRCLE('',#19806,6.00000000000001);
#7626=CIRCLE('',#19809,6.);
#7627=CIRCLE('',#19814,6.00000000000001);
#7628=CIRCLE('',#19818,6.00000000000001);
#7629=CIRCLE('',#19820,6.00000000000001);
#7630=CIRCLE('',#19822,6.);
#7631=CIRCLE('',#19841,12.);
#7632=CIRCLE('',#19843,12.);
#7633=CIRCLE('',#19847,6.);
#7634=CIRCLE('',#19848,6.);
#7635=CIRCLE('',#19851,6.);
#7636=CIRCLE('',#19852,6.);
#7637=CIRCLE('',#19856,12.);
#7638=CIRCLE('',#19858,12.);
#7639=CIRCLE('',#19860,105.377972911614);
#7640=CIRCLE('',#19861,20.5);
#7641=CIRCLE('',#19863,23.5);
#7642=CIRCLE('',#19864,23.5);
#7643=CIRCLE('',#19866,100.);
#7644=CIRCLE('',#19867,100.);
#7645=CIRCLE('',#19868,100.);
#7646=CIRCLE('',#19869,100.);
#7647=CIRCLE('',#19870,20.5);
#7648=CIRCLE('',#19873,106.259607815157);
#7649=CIRCLE('',#19890,12.);
#7650=CIRCLE('',#19892,12.);
#7651=CIRCLE('',#19894,12.);
#7652=CIRCLE('',#19903,12.);
#7653=CIRCLE('',#19905,107.1412427187);
#7654=CIRCLE('',#19907,107.1412427187);
#7655=CIRCLE('',#19909,107.1412427187);
#7656=CIRCLE('',#19911,107.1412427187);
#7657=CIRCLE('',#19946,2.);
#7658=CIRCLE('',#19947,2.);
#7659=CIRCLE('',#19948,0.2);
#7660=CIRCLE('',#19949,2.2);
#7661=CIRCLE('',#19951,3.5);
#7662=CIRCLE('',#19952,3.5);
#7663=CIRCLE('',#19953,3.5);
#7664=CIRCLE('',#19954,3.5);
#7665=CIRCLE('',#19955,3.5);
#7666=CIRCLE('',#19956,3.5);
#7667=CIRCLE('',#19957,3.5);
#7668=CIRCLE('',#19959,2.);
#7669=CIRCLE('',#19960,1.61);
#7670=CIRCLE('',#19971,3.5);
#7671=CIRCLE('',#19972,3.5);
#7672=CIRCLE('',#19973,3.5);
#7673=CIRCLE('',#19974,3.5);
#7674=CIRCLE('',#19975,3.5);
#7675=CIRCLE('',#19976,3.5);
#7676=VERTEX_POINT('',#24908);
#7677=VERTEX_POINT('',#24910);
#7678=VERTEX_POINT('',#24914);
#7679=VERTEX_POINT('',#24915);
#7680=VERTEX_POINT('',#24918);
#7681=VERTEX_POINT('',#24922);
#7682=VERTEX_POINT('',#24923);
#7683=VERTEX_POINT('',#24925);
#7684=VERTEX_POINT('',#24927);
#7685=VERTEX_POINT('',#24929);
#7686=VERTEX_POINT('',#24931);
#7687=VERTEX_POINT('',#24933);
#7688=VERTEX_POINT('',#24935);
#7689=VERTEX_POINT('',#24937);
#7690=VERTEX_POINT('',#24939);
#7691=VERTEX_POINT('',#24941);
#7692=VERTEX_POINT('',#24943);
#7693=VERTEX_POINT('',#24945);
#7694=VERTEX_POINT('',#24947);
#7695=VERTEX_POINT('',#24949);
#7696=VERTEX_POINT('',#24951);
#7697=VERTEX_POINT('',#24953);
#7698=VERTEX_POINT('',#24955);
#7699=VERTEX_POINT('',#24957);
#7700=VERTEX_POINT('',#24960);
#7701=VERTEX_POINT('',#24962);
#7702=VERTEX_POINT('',#24964);
#7703=VERTEX_POINT('',#24966);
#7704=VERTEX_POINT('',#24968);
#7705=VERTEX_POINT('',#24970);
#7706=VERTEX_POINT('',#24972);
#7707=VERTEX_POINT('',#24974);
#7708=VERTEX_POINT('',#24976);
#7709=VERTEX_POINT('',#24978);
#7710=VERTEX_POINT('',#24980);
#7711=VERTEX_POINT('',#24982);
#7712=VERTEX_POINT('',#24984);
#7713=VERTEX_POINT('',#24986);
#7714=VERTEX_POINT('',#24988);
#7715=VERTEX_POINT('',#24990);
#7716=VERTEX_POINT('',#24992);
#7717=VERTEX_POINT('',#24994);
#7718=VERTEX_POINT('',#24996);
#7719=VERTEX_POINT('',#25000);
#7720=VERTEX_POINT('',#25002);
#7721=VERTEX_POINT('',#25006);
#7722=VERTEX_POINT('',#25008);
#7723=VERTEX_POINT('',#25012);
#7724=VERTEX_POINT('',#25014);
#7725=VERTEX_POINT('',#25018);
#7726=VERTEX_POINT('',#25020);
#7727=VERTEX_POINT('',#25024);
#7728=VERTEX_POINT('',#25026);
#7729=VERTEX_POINT('',#25030);
#7730=VERTEX_POINT('',#25032);
#7731=VERTEX_POINT('',#25036);
#7732=VERTEX_POINT('',#25038);
#7733=VERTEX_POINT('',#25042);
#7734=VERTEX_POINT('',#25044);
#7735=VERTEX_POINT('',#25048);
#7736=VERTEX_POINT('',#25111);
#7737=VERTEX_POINT('',#25115);
#7738=VERTEX_POINT('',#25178);
#7739=VERTEX_POINT('',#25182);
#7740=VERTEX_POINT('',#25249);
#7741=VERTEX_POINT('',#25253);
#7742=VERTEX_POINT('',#25320);
#7743=VERTEX_POINT('',#25324);
#7744=VERTEX_POINT('',#25328);
#7745=VERTEX_POINT('',#25330);
#7746=VERTEX_POINT('',#25334);
#7747=VERTEX_POINT('',#25336);
#7748=VERTEX_POINT('',#25340);
#7749=VERTEX_POINT('',#25342);
#7750=VERTEX_POINT('',#25346);
#7751=VERTEX_POINT('',#25348);
#7752=VERTEX_POINT('',#25352);
#7753=VERTEX_POINT('',#25354);
#7754=VERTEX_POINT('',#25358);
#7755=VERTEX_POINT('',#25360);
#7756=VERTEX_POINT('',#25364);
#7757=VERTEX_POINT('',#25366);
#7758=VERTEX_POINT('',#25370);
#7759=VERTEX_POINT('',#25372);
#7760=VERTEX_POINT('',#25376);
#7761=VERTEX_POINT('',#25378);
#7762=VERTEX_POINT('',#25382);
#7763=VERTEX_POINT('',#25384);
#7764=VERTEX_POINT('',#25388);
#7765=VERTEX_POINT('',#25390);
#7766=VERTEX_POINT('',#25394);
#7767=VERTEX_POINT('',#25396);
#7768=VERTEX_POINT('',#25400);
#7769=VERTEX_POINT('',#25402);
#7770=VERTEX_POINT('',#25406);
#7771=VERTEX_POINT('',#25408);
#7772=VERTEX_POINT('',#25412);
#7773=VERTEX_POINT('',#25414);
#7774=VERTEX_POINT('',#25418);
#7775=VERTEX_POINT('',#25422);
#7776=VERTEX_POINT('',#25424);
#7777=VERTEX_POINT('',#25428);
#7778=VERTEX_POINT('',#25430);
#7779=VERTEX_POINT('',#25434);
#7780=VERTEX_POINT('',#25436);
#7781=VERTEX_POINT('',#25438);
#7782=VERTEX_POINT('',#25441);
#7783=VERTEX_POINT('',#25443);
#7784=VERTEX_POINT('',#25446);
#7785=VERTEX_POINT('',#25448);
#7786=VERTEX_POINT('',#25451);
#7787=VERTEX_POINT('',#25453);
#7788=VERTEX_POINT('',#25456);
#7789=VERTEX_POINT('',#25458);
#7790=VERTEX_POINT('',#25461);
#7791=VERTEX_POINT('',#25463);
#7792=VERTEX_POINT('',#25466);
#7793=VERTEX_POINT('',#25468);
#7794=VERTEX_POINT('',#25471);
#7795=VERTEX_POINT('',#25473);
#7796=VERTEX_POINT('',#25476);
#7797=VERTEX_POINT('',#25483);
#7798=VERTEX_POINT('',#25484);
#7799=VERTEX_POINT('',#25486);
#7800=VERTEX_POINT('',#25488);
#7801=VERTEX_POINT('',#25490);
#7802=VERTEX_POINT('',#25492);
#7803=VERTEX_POINT('',#25494);
#7804=VERTEX_POINT('',#25496);
#7805=VERTEX_POINT('',#25500);
#7806=VERTEX_POINT('',#25501);
#7807=VERTEX_POINT('',#25503);
#7808=VERTEX_POINT('',#25505);
#7809=VERTEX_POINT('',#25507);
#7810=VERTEX_POINT('',#25509);
#7811=VERTEX_POINT('',#25511);
#7812=VERTEX_POINT('',#25513);
#7813=VERTEX_POINT('',#25533);
#7814=VERTEX_POINT('',#25534);
#7815=VERTEX_POINT('',#25536);
#7816=VERTEX_POINT('',#25538);
#7817=VERTEX_POINT('',#25540);
#7818=VERTEX_POINT('',#25542);
#7819=VERTEX_POINT('',#25544);
#7820=VERTEX_POINT('',#25546);
#7821=VERTEX_POINT('',#25550);
#7822=VERTEX_POINT('',#25551);
#7823=VERTEX_POINT('',#25553);
#7824=VERTEX_POINT('',#25555);
#7825=VERTEX_POINT('',#25557);
#7826=VERTEX_POINT('',#25559);
#7827=VERTEX_POINT('',#25561);
#7828=VERTEX_POINT('',#25563);
#7829=VERTEX_POINT('',#25630);
#7830=VERTEX_POINT('',#25631);
#7831=VERTEX_POINT('',#25633);
#7832=VERTEX_POINT('',#25635);
#7833=VERTEX_POINT('',#25642);
#7834=VERTEX_POINT('',#25644);
#7835=VERTEX_POINT('',#25646);
#7836=VERTEX_POINT('',#25653);
#7837=VERTEX_POINT('',#25660);
#7838=VERTEX_POINT('',#25670);
#7839=VERTEX_POINT('',#25679);
#7840=VERTEX_POINT('',#25686);
#7841=VERTEX_POINT('',#25695);
#7842=VERTEX_POINT('',#25713);
#7843=VERTEX_POINT('',#25714);
#7844=VERTEX_POINT('',#25716);
#7845=VERTEX_POINT('',#25718);
#7846=VERTEX_POINT('',#25725);
#7847=VERTEX_POINT('',#25726);
#7848=VERTEX_POINT('',#25731);
#7849=VERTEX_POINT('',#25733);
#7850=VERTEX_POINT('',#26141);
#7851=VERTEX_POINT('',#26142);
#7852=VERTEX_POINT('',#26144);
#7853=VERTEX_POINT('',#26146);
#7854=VERTEX_POINT('',#26153);
#7855=VERTEX_POINT('',#26155);
#7856=VERTEX_POINT('',#26157);
#7857=VERTEX_POINT('',#26166);
#7858=VERTEX_POINT('',#26175);
#7859=VERTEX_POINT('',#26182);
#7860=VERTEX_POINT('',#26189);
#7861=VERTEX_POINT('',#26198);
#7862=VERTEX_POINT('',#26208);
#7863=VERTEX_POINT('',#26224);
#7864=VERTEX_POINT('',#26225);
#7865=VERTEX_POINT('',#26227);
#7866=VERTEX_POINT('',#26229);
#7867=VERTEX_POINT('',#26233);
#7868=VERTEX_POINT('',#26237);
#7869=VERTEX_POINT('',#26240);
#7870=VERTEX_POINT('',#26241);
#7871=VERTEX_POINT('',#26246);
#7872=VERTEX_POINT('',#26248);
#7873=VERTEX_POINT('',#26317);
#7874=VERTEX_POINT('',#26319);
#7875=VERTEX_POINT('',#26346);
#7876=VERTEX_POINT('',#26347);
#7877=VERTEX_POINT('',#26349);
#7878=VERTEX_POINT('',#26351);
#7879=VERTEX_POINT('',#26355);
#7880=VERTEX_POINT('',#26356);
#7881=VERTEX_POINT('',#26358);
#7882=VERTEX_POINT('',#26360);
#7883=VERTEX_POINT('',#26387);
#7884=VERTEX_POINT('',#26389);
#7885=VERTEX_POINT('',#26564);
#7886=VERTEX_POINT('',#26565);
#7887=VERTEX_POINT('',#26567);
#7888=VERTEX_POINT('',#26569);
#7889=VERTEX_POINT('',#26573);
#7890=VERTEX_POINT('',#26574);
#7891=VERTEX_POINT('',#26576);
#7892=VERTEX_POINT('',#26578);
#7893=VERTEX_POINT('',#26582);
#7894=VERTEX_POINT('',#26583);
#7895=VERTEX_POINT('',#26585);
#7896=VERTEX_POINT('',#26587);
#7897=VERTEX_POINT('',#26591);
#7898=VERTEX_POINT('',#26594);
#7899=VERTEX_POINT('',#26598);
#7900=VERTEX_POINT('',#26601);
#7901=VERTEX_POINT('',#26606);
#7902=VERTEX_POINT('',#26805);
#7903=VERTEX_POINT('',#26807);
#7904=VERTEX_POINT('',#26810);
#7905=VERTEX_POINT('',#26811);
#7906=VERTEX_POINT('',#26815);
#7907=VERTEX_POINT('',#26817);
#7908=VERTEX_POINT('',#26820);
#7909=VERTEX_POINT('',#26822);
#7910=VERTEX_POINT('',#26826);
#7911=VERTEX_POINT('',#26828);
#7912=VERTEX_POINT('',#26830);
#7913=VERTEX_POINT('',#26834);
#7914=VERTEX_POINT('',#26836);
#7915=VERTEX_POINT('',#26838);
#7916=VERTEX_POINT('',#26841);
#7917=VERTEX_POINT('',#26842);
#7918=VERTEX_POINT('',#26844);
#7919=VERTEX_POINT('',#26846);
#7920=VERTEX_POINT('',#26848);
#7921=VERTEX_POINT('',#26850);
#7922=VERTEX_POINT('',#26853);
#7923=VERTEX_POINT('',#26855);
#7924=VERTEX_POINT('',#26857);
#7925=VERTEX_POINT('',#26859);
#7926=VERTEX_POINT('',#26861);
#7927=VERTEX_POINT('',#26863);
#7928=VERTEX_POINT('',#26865);
#7929=VERTEX_POINT('',#26867);
#7930=VERTEX_POINT('',#26869);
#7931=VERTEX_POINT('',#26871);
#7932=VERTEX_POINT('',#26873);
#7933=VERTEX_POINT('',#26875);
#7934=VERTEX_POINT('',#26877);
#7935=VERTEX_POINT('',#26879);
#7936=VERTEX_POINT('',#26881);
#7937=VERTEX_POINT('',#26883);
#7938=VERTEX_POINT('',#26885);
#7939=VERTEX_POINT('',#26887);
#7940=VERTEX_POINT('',#26889);
#7941=VERTEX_POINT('',#26891);
#7942=VERTEX_POINT('',#26893);
#7943=VERTEX_POINT('',#26895);
#7944=VERTEX_POINT('',#26897);
#7945=VERTEX_POINT('',#26899);
#7946=VERTEX_POINT('',#26901);
#7947=VERTEX_POINT('',#26903);
#7948=VERTEX_POINT('',#26905);
#7949=VERTEX_POINT('',#26907);
#7950=VERTEX_POINT('',#26909);
#7951=VERTEX_POINT('',#26911);
#7952=VERTEX_POINT('',#26913);
#7953=VERTEX_POINT('',#26917);
#7954=VERTEX_POINT('',#26919);
#7955=VERTEX_POINT('',#26923);
#7956=VERTEX_POINT('',#26925);
#7957=VERTEX_POINT('',#26929);
#7958=VERTEX_POINT('',#26931);
#7959=VERTEX_POINT('',#26935);
#7960=VERTEX_POINT('',#26937);
#7961=VERTEX_POINT('',#26941);
#7962=VERTEX_POINT('',#26943);
#7963=VERTEX_POINT('',#26947);
#7964=VERTEX_POINT('',#26949);
#7965=VERTEX_POINT('',#26953);
#7966=VERTEX_POINT('',#26955);
#7967=VERTEX_POINT('',#26959);
#7968=VERTEX_POINT('',#26961);
#7969=VERTEX_POINT('',#26967);
#7970=VERTEX_POINT('',#26969);
#7971=VERTEX_POINT('',#26973);
#7972=VERTEX_POINT('',#26979);
#7973=VERTEX_POINT('',#26983);
#7974=VERTEX_POINT('',#26987);
#7975=VERTEX_POINT('',#26994);
#7976=VERTEX_POINT('',#26996);
#7977=VERTEX_POINT('',#27000);
#7978=VERTEX_POINT('',#27002);
#7979=VERTEX_POINT('',#27005);
#7980=VERTEX_POINT('',#27007);
#7981=VERTEX_POINT('',#27010);
#7982=VERTEX_POINT('',#27012);
#7983=VERTEX_POINT('',#27015);
#7984=VERTEX_POINT('',#27017);
#7985=VERTEX_POINT('',#27019);
#7986=VERTEX_POINT('',#27021);
#7987=VERTEX_POINT('',#27024);
#7988=VERTEX_POINT('',#27026);
#7989=VERTEX_POINT('',#27028);
#7990=VERTEX_POINT('',#27031);
#7991=VERTEX_POINT('',#27033);
#7992=VERTEX_POINT('',#27036);
#7993=VERTEX_POINT('',#27038);
#7994=VERTEX_POINT('',#27041);
#7995=VERTEX_POINT('',#27043);
#7996=VERTEX_POINT('',#27046);
#7997=VERTEX_POINT('',#27048);
#7998=VERTEX_POINT('',#27051);
#7999=VERTEX_POINT('',#27053);
#8000=VERTEX_POINT('',#27161);
#8001=VERTEX_POINT('',#27162);
#8002=VERTEX_POINT('',#27164);
#8003=VERTEX_POINT('',#27166);
#8004=VERTEX_POINT('',#27267);
#8005=VERTEX_POINT('',#27346);
#8006=VERTEX_POINT('',#27348);
#8007=VERTEX_POINT('',#27351);
#8008=VERTEX_POINT('',#27448);
#8009=VERTEX_POINT('',#27449);
#8010=VERTEX_POINT('',#27452);
#8011=VERTEX_POINT('',#27454);
#8012=VERTEX_POINT('',#27531);
#8013=VERTEX_POINT('',#27629);
#8014=VERTEX_POINT('',#27631);
#8015=VERTEX_POINT('',#27634);
#8016=VERTEX_POINT('',#28102);
#8017=VERTEX_POINT('',#28103);
#8018=VERTEX_POINT('',#28378);
#8019=VERTEX_POINT('',#28382);
#8020=VERTEX_POINT('',#28691);
#8021=VERTEX_POINT('',#28692);
#8022=VERTEX_POINT('',#29075);
#8023=VERTEX_POINT('',#29079);
#8024=VERTEX_POINT('',#30302);
#8025=VERTEX_POINT('',#30304);
#8026=VERTEX_POINT('',#30308);
#8027=VERTEX_POINT('',#30310);
#8028=VERTEX_POINT('',#30314);
#8029=VERTEX_POINT('',#30316);
#8030=VERTEX_POINT('',#30320);
#8031=VERTEX_POINT('',#30322);
#8032=VERTEX_POINT('',#30326);
#8033=VERTEX_POINT('',#30327);
#8034=VERTEX_POINT('',#30329);
#8035=VERTEX_POINT('',#30331);
#8036=VERTEX_POINT('',#30333);
#8037=VERTEX_POINT('',#30335);
#8038=VERTEX_POINT('',#30337);
#8039=VERTEX_POINT('',#30339);
#8040=VERTEX_POINT('',#30341);
#8041=VERTEX_POINT('',#30343);
#8042=VERTEX_POINT('',#30345);
#8043=VERTEX_POINT('',#30347);
#8044=VERTEX_POINT('',#30351);
#8045=VERTEX_POINT('',#30352);
#8046=VERTEX_POINT('',#30354);
#8047=VERTEX_POINT('',#30356);
#8048=VERTEX_POINT('',#30358);
#8049=VERTEX_POINT('',#30360);
#8050=VERTEX_POINT('',#30362);
#8051=VERTEX_POINT('',#30364);
#8052=VERTEX_POINT('',#30366);
#8053=VERTEX_POINT('',#30368);
#8054=VERTEX_POINT('',#30370);
#8055=VERTEX_POINT('',#30372);
#8056=VERTEX_POINT('',#30376);
#8057=VERTEX_POINT('',#30378);
#8058=VERTEX_POINT('',#30382);
#8059=VERTEX_POINT('',#30384);
#8060=VERTEX_POINT('',#30388);
#8061=VERTEX_POINT('',#30390);
#8062=VERTEX_POINT('',#30394);
#8063=VERTEX_POINT('',#30396);
#8064=VERTEX_POINT('',#30403);
#8065=VERTEX_POINT('',#30405);
#8066=VERTEX_POINT('',#30409);
#8067=VERTEX_POINT('',#30411);
#8068=VERTEX_POINT('',#30415);
#8069=VERTEX_POINT('',#30417);
#8070=VERTEX_POINT('',#30421);
#8071=VERTEX_POINT('',#30423);
#8072=VERTEX_POINT('',#30431);
#8073=VERTEX_POINT('',#30433);
#8074=VERTEX_POINT('',#30436);
#8075=VERTEX_POINT('',#30438);
#8076=VERTEX_POINT('',#30442);
#8077=VERTEX_POINT('',#30446);
#8078=VERTEX_POINT('',#30451);
#8079=VERTEX_POINT('',#30453);
#8080=VERTEX_POINT('',#30455);
#8081=VERTEX_POINT('',#30459);
#8082=VERTEX_POINT('',#30463);
#8083=VERTEX_POINT('',#30467);
#8084=VERTEX_POINT('',#30474);
#8085=VERTEX_POINT('',#30478);
#8086=VERTEX_POINT('',#30491);
#8087=VERTEX_POINT('',#30493);
#8088=VERTEX_POINT('',#30497);
#8089=VERTEX_POINT('',#30499);
#8090=VERTEX_POINT('',#30503);
#8091=VERTEX_POINT('',#30505);
#8092=VERTEX_POINT('',#30509);
#8093=VERTEX_POINT('',#30511);
#8094=VERTEX_POINT('',#30515);
#8095=VERTEX_POINT('',#30517);
#8096=VERTEX_POINT('',#30521);
#8097=VERTEX_POINT('',#30523);
#8098=VERTEX_POINT('',#30527);
#8099=VERTEX_POINT('',#30529);
#8100=VERTEX_POINT('',#30533);
#8101=VERTEX_POINT('',#30535);
#8102=VERTEX_POINT('',#30539);
#8103=VERTEX_POINT('',#30541);
#8104=VERTEX_POINT('',#30545);
#8105=VERTEX_POINT('',#30547);
#8106=VERTEX_POINT('',#30551);
#8107=VERTEX_POINT('',#30553);
#8108=VERTEX_POINT('',#30557);
#8109=VERTEX_POINT('',#30559);
#8110=VERTEX_POINT('',#30563);
#8111=VERTEX_POINT('',#30565);
#8112=VERTEX_POINT('',#30569);
#8113=VERTEX_POINT('',#30571);
#8114=VERTEX_POINT('',#30575);
#8115=VERTEX_POINT('',#30577);
#8116=VERTEX_POINT('',#30581);
#8117=VERTEX_POINT('',#30583);
#8118=VERTEX_POINT('',#30587);
#8119=VERTEX_POINT('',#30589);
#8120=VERTEX_POINT('',#30595);
#8121=VERTEX_POINT('',#30597);
#8122=VERTEX_POINT('',#30604);
#8123=VERTEX_POINT('',#30606);
#8124=VERTEX_POINT('',#30608);
#8125=VERTEX_POINT('',#30612);
#8126=VERTEX_POINT('',#30613);
#8127=VERTEX_POINT('',#30615);
#8128=VERTEX_POINT('',#30617);
#8129=VERTEX_POINT('',#30622);
#8130=VERTEX_POINT('',#30623);
#8131=VERTEX_POINT('',#30625);
#8132=VERTEX_POINT('',#30627);
#8133=VERTEX_POINT('',#30632);
#8134=VERTEX_POINT('',#30633);
#8135=VERTEX_POINT('',#30635);
#8136=VERTEX_POINT('',#30637);
#8137=VERTEX_POINT('',#30642);
#8138=VERTEX_POINT('',#30644);
#8139=VERTEX_POINT('',#30650);
#8140=VERTEX_POINT('',#30660);
#8141=VERTEX_POINT('',#30661);
#8142=VERTEX_POINT('',#30664);
#8143=VERTEX_POINT('',#30668);
#8144=VERTEX_POINT('',#30673);
#8145=VERTEX_POINT('',#30674);
#8146=VERTEX_POINT('',#30679);
#8147=VERTEX_POINT('',#30680);
#8148=VERTEX_POINT('',#30682);
#8149=VERTEX_POINT('',#30684);
#8150=VERTEX_POINT('',#30686);
#8151=VERTEX_POINT('',#30688);
#8152=VERTEX_POINT('',#30692);
#8153=VERTEX_POINT('',#30694);
#8154=VERTEX_POINT('',#30698);
#8155=VERTEX_POINT('',#30702);
#8156=VERTEX_POINT('',#30704);
#8157=VERTEX_POINT('',#30708);
#8158=VERTEX_POINT('',#30712);
#8159=VERTEX_POINT('',#30716);
#8160=VERTEX_POINT('',#30730);
#8161=VERTEX_POINT('',#30731);
#8162=VERTEX_POINT('',#30736);
#8163=VERTEX_POINT('',#30738);
#8164=VERTEX_POINT('',#30745);
#8165=VERTEX_POINT('',#30761);
#8166=VERTEX_POINT('',#30766);
#8167=VERTEX_POINT('',#30768);
#8168=VERTEX_POINT('',#30775);
#8169=VERTEX_POINT('',#30789);
#8170=VERTEX_POINT('',#30791);
#8171=VERTEX_POINT('',#30793);
#8172=VERTEX_POINT('',#30797);
#8173=VERTEX_POINT('',#30799);
#8174=VERTEX_POINT('',#30803);
#8175=VERTEX_POINT('',#30805);
#8176=VERTEX_POINT('',#30809);
#8177=VERTEX_POINT('',#30811);
#8178=VERTEX_POINT('',#30815);
#8179=VERTEX_POINT('',#30817);
#8180=VERTEX_POINT('',#30821);
#8181=VERTEX_POINT('',#30822);
#8182=VERTEX_POINT('',#30824);
#8183=VERTEX_POINT('',#30826);
#8184=VERTEX_POINT('',#30831);
#8185=VERTEX_POINT('',#30832);
#8186=VERTEX_POINT('',#30834);
#8187=VERTEX_POINT('',#30839);
#8188=VERTEX_POINT('',#30846);
#8189=VERTEX_POINT('',#30847);
#8190=VERTEX_POINT('',#30849);
#8191=VERTEX_POINT('',#30858);
#8192=VERTEX_POINT('',#30860);
#8193=VERTEX_POINT('',#30866);
#8194=VERTEX_POINT('',#30875);
#8195=VERTEX_POINT('',#30877);
#8196=VERTEX_POINT('',#30884);
#8197=VERTEX_POINT('',#30886);
#8198=VERTEX_POINT('',#30890);
#8199=VERTEX_POINT('',#30892);
#8200=VERTEX_POINT('',#30894);
#8201=VERTEX_POINT('',#30901);
#8202=VERTEX_POINT('',#30903);
#8203=VERTEX_POINT('',#30910);
#8204=VERTEX_POINT('',#30912);
#8205=VERTEX_POINT('',#30919);
#8206=VERTEX_POINT('',#30928);
#8207=VERTEX_POINT('',#30929);
#8208=VERTEX_POINT('',#30931);
#8209=VERTEX_POINT('',#30933);
#8210=VERTEX_POINT('',#30935);
#8211=VERTEX_POINT('',#30938);
#8212=VERTEX_POINT('',#30942);
#8213=VERTEX_POINT('',#30944);
#8214=VERTEX_POINT('',#30948);
#8215=VERTEX_POINT('',#30950);
#8216=VERTEX_POINT('',#30954);
#8217=VERTEX_POINT('',#30955);
#8218=VERTEX_POINT('',#30974);
#8219=VERTEX_POINT('',#30976);
#8220=VERTEX_POINT('',#30997);
#8221=VERTEX_POINT('',#30998);
#8222=VERTEX_POINT('',#31017);
#8223=VERTEX_POINT('',#31019);
#8224=VERTEX_POINT('',#31040);
#8225=VERTEX_POINT('',#31041);
#8226=VERTEX_POINT('',#31043);
#8227=VERTEX_POINT('',#31050);
#8228=VERTEX_POINT('',#31052);
#8229=VERTEX_POINT('',#31059);
#8230=VERTEX_POINT('',#31061);
#8231=VERTEX_POINT('',#31070);
#8232=VERTEX_POINT('',#31081);
#8233=VERTEX_POINT('',#31082);
#8234=VERTEX_POINT('',#31101);
#8235=VERTEX_POINT('',#31103);
#8236=VERTEX_POINT('',#31107);
#8237=VERTEX_POINT('',#31108);
#8238=VERTEX_POINT('',#31127);
#8239=VERTEX_POINT('',#31129);
#8240=VERTEX_POINT('',#31150);
#8241=VERTEX_POINT('',#31151);
#8242=VERTEX_POINT('',#31153);
#8243=VERTEX_POINT('',#31155);
#8244=VERTEX_POINT('',#31157);
#8245=VERTEX_POINT('',#31161);
#8246=VERTEX_POINT('',#31163);
#8247=VERTEX_POINT('',#31167);
#8248=VERTEX_POINT('',#31169);
#8249=VERTEX_POINT('',#31173);
#8250=VERTEX_POINT('',#31175);
#8251=VERTEX_POINT('',#31179);
#8252=VERTEX_POINT('',#31181);
#8253=VERTEX_POINT('',#31185);
#8254=VERTEX_POINT('',#31187);
#8255=VERTEX_POINT('',#31191);
#8256=VERTEX_POINT('',#31192);
#8257=VERTEX_POINT('',#31194);
#8258=VERTEX_POINT('',#31196);
#8259=VERTEX_POINT('',#31217);
#8260=VERTEX_POINT('',#31218);
#8261=VERTEX_POINT('',#31220);
#8262=VERTEX_POINT('',#31222);
#8263=VERTEX_POINT('',#31245);
#8264=VERTEX_POINT('',#31247);
#8265=VERTEX_POINT('',#31249);
#8266=VERTEX_POINT('',#31251);
#8267=VERTEX_POINT('',#31266);
#8268=VERTEX_POINT('',#31267);
#8269=VERTEX_POINT('',#31269);
#8270=VERTEX_POINT('',#31273);
#8271=VERTEX_POINT('',#31275);
#8272=VERTEX_POINT('',#31279);
#8273=VERTEX_POINT('',#31281);
#8274=VERTEX_POINT('',#31285);
#8275=VERTEX_POINT('',#31287);
#8276=VERTEX_POINT('',#31291);
#8277=VERTEX_POINT('',#31294);
#8278=VERTEX_POINT('',#31298);
#8279=VERTEX_POINT('',#31305);
#8280=VERTEX_POINT('',#31307);
#8281=VERTEX_POINT('',#31311);
#8282=VERTEX_POINT('',#31313);
#8283=VERTEX_POINT('',#31317);
#8284=VERTEX_POINT('',#31319);
#8285=VERTEX_POINT('',#31323);
#8286=VERTEX_POINT('',#31328);
#8287=VERTEX_POINT('',#31329);
#8288=VERTEX_POINT('',#31361);
#8289=VERTEX_POINT('',#31362);
#8290=VERTEX_POINT('',#31364);
#8291=VERTEX_POINT('',#31366);
#8292=VERTEX_POINT('',#31372);
#8293=VERTEX_POINT('',#31373);
#8294=VERTEX_POINT('',#31375);
#8295=VERTEX_POINT('',#31377);
#8296=VERTEX_POINT('',#31381);
#8297=VERTEX_POINT('',#31382);
#8298=VERTEX_POINT('',#31384);
#8299=VERTEX_POINT('',#31386);
#8300=VERTEX_POINT('',#31389);
#8301=VERTEX_POINT('',#31391);
#8302=VERTEX_POINT('',#31395);
#8303=VERTEX_POINT('',#31399);
#8304=VERTEX_POINT('',#31401);
#8305=VERTEX_POINT('',#31405);
#8306=VERTEX_POINT('',#31407);
#8307=VERTEX_POINT('',#31411);
#8308=VERTEX_POINT('',#31413);
#8309=VERTEX_POINT('',#31417);
#8310=VERTEX_POINT('',#31419);
#8311=VERTEX_POINT('',#31423);
#8312=VERTEX_POINT('',#31425);
#8313=VERTEX_POINT('',#31427);
#8314=VERTEX_POINT('',#31429);
#8315=VERTEX_POINT('',#31431);
#8316=VERTEX_POINT('',#31433);
#8317=VERTEX_POINT('',#31436);
#8318=VERTEX_POINT('',#31438);
#8319=VERTEX_POINT('',#31442);
#8320=VERTEX_POINT('',#31444);
#8321=VERTEX_POINT('',#31448);
#8322=VERTEX_POINT('',#31450);
#8323=VERTEX_POINT('',#31454);
#8324=VERTEX_POINT('',#31458);
#8325=VERTEX_POINT('',#31460);
#8326=VERTEX_POINT('',#31464);
#8327=VERTEX_POINT('',#31466);
#8328=VERTEX_POINT('',#31470);
#8329=VERTEX_POINT('',#31472);
#8330=VERTEX_POINT('',#31476);
#8331=VERTEX_POINT('',#31478);
#8332=VERTEX_POINT('',#31482);
#8333=VERTEX_POINT('',#31484);
#8334=VERTEX_POINT('',#31488);
#8335=VERTEX_POINT('',#31490);
#8336=VERTEX_POINT('',#31494);
#8337=VERTEX_POINT('',#31495);
#8338=VERTEX_POINT('',#31497);
#8339=VERTEX_POINT('',#31499);
#8340=VERTEX_POINT('',#31503);
#8341=VERTEX_POINT('',#31505);
#8342=VERTEX_POINT('',#31509);
#8343=VERTEX_POINT('',#31510);
#8344=VERTEX_POINT('',#31512);
#8345=VERTEX_POINT('',#31514);
#8346=VERTEX_POINT('',#31518);
#8347=VERTEX_POINT('',#31519);
#8348=VERTEX_POINT('',#31524);
#8349=VERTEX_POINT('',#31525);
#8350=VERTEX_POINT('',#31530);
#8351=VERTEX_POINT('',#31531);
#8352=VERTEX_POINT('',#31542);
#8353=VERTEX_POINT('',#31549);
#8354=VERTEX_POINT('',#31551);
#8355=VERTEX_POINT('',#31558);
#8356=VERTEX_POINT('',#31569);
#8357=VERTEX_POINT('',#31576);
#8358=VERTEX_POINT('',#31578);
#8359=VERTEX_POINT('',#31585);
#8360=VERTEX_POINT('',#31592);
#8361=VERTEX_POINT('',#31594);
#8362=VERTEX_POINT('',#31596);
#8363=VERTEX_POINT('',#31598);
#8364=VERTEX_POINT('',#31605);
#8365=VERTEX_POINT('',#31612);
#8366=VERTEX_POINT('',#31614);
#8367=VERTEX_POINT('',#31621);
#8368=VERTEX_POINT('',#31630);
#8369=VERTEX_POINT('',#31637);
#8370=VERTEX_POINT('',#31646);
#8371=VERTEX_POINT('',#31648);
#8372=VERTEX_POINT('',#31652);
#8373=VERTEX_POINT('',#31654);
#8374=VERTEX_POINT('',#31658);
#8375=VERTEX_POINT('',#31662);
#8376=VERTEX_POINT('',#31664);
#8377=VERTEX_POINT('',#31666);
#8378=VERTEX_POINT('',#31670);
#8379=VERTEX_POINT('',#31671);
#8380=VERTEX_POINT('',#31673);
#8381=VERTEX_POINT('',#31675);
#8382=VERTEX_POINT('',#31679);
#8383=VERTEX_POINT('',#31689);
#8384=VERTEX_POINT('',#31690);
#8385=VERTEX_POINT('',#31729);
#8386=VERTEX_POINT('',#31731);
#8387=VERTEX_POINT('',#31784);
#8388=VERTEX_POINT('',#31785);
#8389=VERTEX_POINT('',#31801);
#8390=VERTEX_POINT('',#31802);
#8391=VERTEX_POINT('',#31804);
#8392=VERTEX_POINT('',#31811);
#8393=VERTEX_POINT('',#31839);
#8394=VERTEX_POINT('',#31861);
#8395=VERTEX_POINT('',#31863);
#8396=VERTEX_POINT('',#31865);
#8397=VERTEX_POINT('',#31914);
#8398=VERTEX_POINT('',#31915);
#8399=VERTEX_POINT('',#31935);
#8400=VERTEX_POINT('',#31937);
#8401=VERTEX_POINT('',#31939);
#8402=VERTEX_POINT('',#31988);
#8403=VERTEX_POINT('',#31989);
#8404=VERTEX_POINT('',#32009);
#8405=VERTEX_POINT('',#32010);
#8406=VERTEX_POINT('',#32023);
#8407=VERTEX_POINT('',#32024);
#8408=VERTEX_POINT('',#32026);
#8409=VERTEX_POINT('',#32028);
#8410=VERTEX_POINT('',#32030);
#8411=VERTEX_POINT('',#32032);
#8412=VERTEX_POINT('',#32036);
#8413=VERTEX_POINT('',#32037);
#8414=VERTEX_POINT('',#32039);
#8415=VERTEX_POINT('',#32041);
#8416=VERTEX_POINT('',#32043);
#8417=VERTEX_POINT('',#32045);
#8418=VERTEX_POINT('',#32049);
#8419=VERTEX_POINT('',#32050);
#8420=VERTEX_POINT('',#32052);
#8421=VERTEX_POINT('',#32054);
#8422=VERTEX_POINT('',#32056);
#8423=VERTEX_POINT('',#32058);
#8424=VERTEX_POINT('',#32062);
#8425=VERTEX_POINT('',#32063);
#8426=VERTEX_POINT('',#32065);
#8427=VERTEX_POINT('',#32067);
#8428=VERTEX_POINT('',#32069);
#8429=VERTEX_POINT('',#32071);
#8430=VERTEX_POINT('',#32075);
#8431=VERTEX_POINT('',#32076);
#8432=VERTEX_POINT('',#32078);
#8433=VERTEX_POINT('',#32080);
#8434=VERTEX_POINT('',#32082);
#8435=VERTEX_POINT('',#32084);
#8436=VERTEX_POINT('',#32086);
#8437=VERTEX_POINT('',#32089);
#8438=VERTEX_POINT('',#32091);
#8439=VERTEX_POINT('',#32093);
#8440=VERTEX_POINT('',#32095);
#8441=VERTEX_POINT('',#32097);
#8442=VERTEX_POINT('',#32099);
#8443=VERTEX_POINT('',#32101);
#8444=VERTEX_POINT('',#32105);
#8445=VERTEX_POINT('',#32106);
#8446=VERTEX_POINT('',#32108);
#8447=VERTEX_POINT('',#32110);
#8448=VERTEX_POINT('',#32112);
#8449=VERTEX_POINT('',#32114);
#8450=VERTEX_POINT('',#32118);
#8451=VERTEX_POINT('',#32119);
#8452=VERTEX_POINT('',#32121);
#8453=VERTEX_POINT('',#32123);
#8454=VERTEX_POINT('',#32125);
#8455=VERTEX_POINT('',#32127);
#8456=VERTEX_POINT('',#32131);
#8457=VERTEX_POINT('',#32132);
#8458=VERTEX_POINT('',#32137);
#8459=VERTEX_POINT('',#32141);
#8460=VERTEX_POINT('',#32145);
#8461=VERTEX_POINT('',#32149);
#8462=VERTEX_POINT('',#32155);
#8463=VERTEX_POINT('',#32156);
#8464=VERTEX_POINT('',#32158);
#8465=VERTEX_POINT('',#32160);
#8466=VERTEX_POINT('',#32162);
#8467=VERTEX_POINT('',#32166);
#8468=VERTEX_POINT('',#32167);
#8469=VERTEX_POINT('',#32172);
#8470=VERTEX_POINT('',#32174);
#8471=VERTEX_POINT('',#32176);
#8472=VERTEX_POINT('',#32180);
#8473=VERTEX_POINT('',#32181);
#8474=VERTEX_POINT('',#32186);
#8475=VERTEX_POINT('',#32190);
#8476=VERTEX_POINT('',#32194);
#8477=VERTEX_POINT('',#32198);
#8478=VERTEX_POINT('',#32204);
#8479=VERTEX_POINT('',#32205);
#8480=VERTEX_POINT('',#32207);
#8481=VERTEX_POINT('',#32209);
#8482=VERTEX_POINT('',#32211);
#8483=VERTEX_POINT('',#32215);
#8484=VERTEX_POINT('',#32216);
#8485=VERTEX_POINT('',#32221);
#8486=VERTEX_POINT('',#32222);
#8487=VERTEX_POINT('',#32225);
#8488=VERTEX_POINT('',#32229);
#8489=VERTEX_POINT('',#32230);
#8490=VERTEX_POINT('',#32235);
#8491=VERTEX_POINT('',#32239);
#8492=VERTEX_POINT('',#32243);
#8493=VERTEX_POINT('',#32247);
#8494=VERTEX_POINT('',#32253);
#8495=VERTEX_POINT('',#32254);
#8496=VERTEX_POINT('',#32256);
#8497=VERTEX_POINT('',#32258);
#8498=VERTEX_POINT('',#32260);
#8499=VERTEX_POINT('',#32264);
#8500=VERTEX_POINT('',#32265);
#8501=VERTEX_POINT('',#32270);
#8502=VERTEX_POINT('',#32271);
#8503=VERTEX_POINT('',#32274);
#8504=VERTEX_POINT('',#32279);
#8505=VERTEX_POINT('',#32281);
#8506=VERTEX_POINT('',#32283);
#8507=VERTEX_POINT('',#32285);
#8508=VERTEX_POINT('',#32290);
#8509=VERTEX_POINT('',#32291);
#8510=VERTEX_POINT('',#32296);
#8511=VERTEX_POINT('',#32300);
#8512=VERTEX_POINT('',#32304);
#8513=VERTEX_POINT('',#32308);
#8514=VERTEX_POINT('',#32314);
#8515=VERTEX_POINT('',#32316);
#8516=VERTEX_POINT('',#32318);
#8517=VERTEX_POINT('',#32322);
#8518=VERTEX_POINT('',#32326);
#8519=VERTEX_POINT('',#32327);
#8520=VERTEX_POINT('',#32332);
#8521=VERTEX_POINT('',#32334);
#8522=VERTEX_POINT('',#32338);
#8523=VERTEX_POINT('',#32342);
#8524=VERTEX_POINT('',#32346);
#8525=VERTEX_POINT('',#32350);
#8526=VERTEX_POINT('',#32354);
#8527=VERTEX_POINT('',#32358);
#8528=VERTEX_POINT('',#32362);
#8529=VERTEX_POINT('',#32366);
#8530=VERTEX_POINT('',#32370);
#8531=VERTEX_POINT('',#32376);
#8532=VERTEX_POINT('',#32380);
#8533=VERTEX_POINT('',#32384);
#8534=VERTEX_POINT('',#32390);
#8535=VERTEX_POINT('',#32392);
#8536=VERTEX_POINT('',#32396);
#8537=VERTEX_POINT('',#32400);
#8538=VERTEX_POINT('',#32404);
#8539=VERTEX_POINT('',#32408);
#8540=VERTEX_POINT('',#32414);
#8541=VERTEX_POINT('',#32416);
#8542=VERTEX_POINT('',#32420);
#8543=VERTEX_POINT('',#32424);
#8544=VERTEX_POINT('',#32428);
#8545=VERTEX_POINT('',#32432);
#8546=VERTEX_POINT('',#32442);
#8547=VERTEX_POINT('',#32443);
#8548=VERTEX_POINT('',#32450);
#8549=VERTEX_POINT('',#32452);
#8550=VERTEX_POINT('',#32456);
#8551=VERTEX_POINT('',#32458);
#8552=VERTEX_POINT('',#32464);
#8553=VERTEX_POINT('',#32466);
#8554=VERTEX_POINT('',#32470);
#8555=VERTEX_POINT('',#32471);
#8556=VERTEX_POINT('',#32478);
#8557=VERTEX_POINT('',#32480);
#8558=VERTEX_POINT('',#32489);
#8559=VERTEX_POINT('',#32491);
#8560=VERTEX_POINT('',#32500);
#8561=VERTEX_POINT('',#32502);
#8562=VERTEX_POINT('',#32516);
#8563=VERTEX_POINT('',#32518);
#8564=VERTEX_POINT('',#32527);
#8565=VERTEX_POINT('',#32529);
#8566=VERTEX_POINT('',#32546);
#8567=VERTEX_POINT('',#32550);
#8568=VERTEX_POINT('',#32556);
#8569=VERTEX_POINT('',#32557);
#8570=VERTEX_POINT('',#32568);
#8571=VERTEX_POINT('',#32570);
#8572=VERTEX_POINT('',#32579);
#8573=VERTEX_POINT('',#32581);
#8574=VERTEX_POINT('',#32590);
#8575=VERTEX_POINT('',#32597);
#8576=VERTEX_POINT('',#32606);
#8577=VERTEX_POINT('',#32607);
#8578=VERTEX_POINT('',#32625);
#8579=VERTEX_POINT('',#32627);
#8580=VERTEX_POINT('',#32634);
#8581=VERTEX_POINT('',#32641);
#8582=VERTEX_POINT('',#32648);
#8583=VERTEX_POINT('',#32655);
#8584=VERTEX_POINT('',#32681);
#8585=VERTEX_POINT('',#32683);
#8586=VERTEX_POINT('',#32690);
#8587=VERTEX_POINT('',#32697);
#8588=VERTEX_POINT('',#32704);
#8589=VERTEX_POINT('',#32711);
#8590=VERTEX_POINT('',#32718);
#8591=VERTEX_POINT('',#32725);
#8592=VERTEX_POINT('',#32732);
#8593=VERTEX_POINT('',#32738);
#8594=VERTEX_POINT('',#32743);
#8595=VERTEX_POINT('',#32745);
#8596=VERTEX_POINT('',#32752);
#8597=VERTEX_POINT('',#32759);
#8598=VERTEX_POINT('',#32766);
#8599=VERTEX_POINT('',#32773);
#8600=VERTEX_POINT('',#32780);
#8601=VERTEX_POINT('',#32787);
#8602=VERTEX_POINT('',#32794);
#8603=VERTEX_POINT('',#32802);
#8604=VERTEX_POINT('',#32830);
#8605=VERTEX_POINT('',#32832);
#8606=VERTEX_POINT('',#32841);
#8607=VERTEX_POINT('',#32850);
#8608=VERTEX_POINT('',#32857);
#8609=VERTEX_POINT('',#32866);
#8610=VERTEX_POINT('',#32885);
#8611=VERTEX_POINT('',#32886);
#8612=VERTEX_POINT('',#32891);
#8613=VERTEX_POINT('',#32895);
#8614=VERTEX_POINT('',#32899);
#8615=VERTEX_POINT('',#32903);
#8616=VERTEX_POINT('',#32907);
#8617=VERTEX_POINT('',#32911);
#8618=VERTEX_POINT('',#33018);
#8619=VERTEX_POINT('',#33034);
#8620=VERTEX_POINT('',#33035);
#8621=VERTEX_POINT('',#33057);
#8622=VERTEX_POINT('',#33073);
#8623=VERTEX_POINT('',#33084);
#8624=VERTEX_POINT('',#33085);
#8625=VERTEX_POINT('',#33101);
#8626=VERTEX_POINT('',#33123);
#8627=VERTEX_POINT('',#33136);
#8628=VERTEX_POINT('',#33137);
#8629=VERTEX_POINT('',#33153);
#8630=VERTEX_POINT('',#33175);
#8631=VERTEX_POINT('',#33188);
#8632=VERTEX_POINT('',#33189);
#8633=VERTEX_POINT('',#33205);
#8634=VERTEX_POINT('',#33543);
#8635=VERTEX_POINT('',#33555);
#8636=VERTEX_POINT('',#33556);
#8637=VERTEX_POINT('',#33634);
#8638=VERTEX_POINT('',#33706);
#8639=VERTEX_POINT('',#33715);
#8640=VERTEX_POINT('',#33716);
#8641=VERTEX_POINT('',#33788);
#8642=VERTEX_POINT('',#33866);
#8643=VERTEX_POINT('',#33875);
#8644=VERTEX_POINT('',#33876);
#8645=VERTEX_POINT('',#33948);
#8646=VERTEX_POINT('',#34026);
#8647=VERTEX_POINT('',#34035);
#8648=VERTEX_POINT('',#34036);
#8649=VERTEX_POINT('',#34108);
#8650=VERTEX_POINT('',#34167);
#8651=VERTEX_POINT('',#35883);
#8652=VERTEX_POINT('',#35966);
#8653=VERTEX_POINT('',#35989);
#8654=VERTEX_POINT('',#35990);
#8655=VERTEX_POINT('',#36014);
#8656=VERTEX_POINT('',#36043);
#8657=VERTEX_POINT('',#36059);
#8658=VERTEX_POINT('',#36060);
#8659=VERTEX_POINT('',#36077);
#8660=VERTEX_POINT('',#36093);
#8661=VERTEX_POINT('',#36106);
#8662=VERTEX_POINT('',#36107);
#8663=VERTEX_POINT('',#36123);
#8664=VERTEX_POINT('',#36145);
#8665=VERTEX_POINT('',#36158);
#8666=VERTEX_POINT('',#36159);
#8667=VERTEX_POINT('',#36175);
#8668=VERTEX_POINT('',#36197);
#8669=VERTEX_POINT('',#36230);
#8670=VERTEX_POINT('',#36231);
#8671=VERTEX_POINT('',#36233);
#8672=VERTEX_POINT('',#36235);
#8673=VERTEX_POINT('',#36237);
#8674=VERTEX_POINT('',#36239);
#8675=VERTEX_POINT('',#36241);
#8676=VERTEX_POINT('',#36243);
#8677=VERTEX_POINT('',#36247);
#8678=VERTEX_POINT('',#36248);
#8679=VERTEX_POINT('',#36253);
#8680=VERTEX_POINT('',#36257);
#8681=VERTEX_POINT('',#36261);
#8682=VERTEX_POINT('',#36265);
#8683=VERTEX_POINT('',#36269);
#8684=VERTEX_POINT('',#36275);
#8685=VERTEX_POINT('',#36279);
#8686=VERTEX_POINT('',#36283);
#8687=VERTEX_POINT('',#36290);
#8688=VERTEX_POINT('',#36294);
#8689=VERTEX_POINT('',#36298);
#8690=VERTEX_POINT('',#36302);
#8691=VERTEX_POINT('',#36308);
#8692=VERTEX_POINT('',#36310);
#8693=VERTEX_POINT('',#36314);
#8694=VERTEX_POINT('',#36316);
#8695=VERTEX_POINT('',#36320);
#8696=VERTEX_POINT('',#36327);
#8697=VERTEX_POINT('',#36336);
#8698=VERTEX_POINT('',#36338);
#8699=VERTEX_POINT('',#36342);
#8700=VERTEX_POINT('',#36349);
#8701=VERTEX_POINT('',#36358);
#8702=VERTEX_POINT('',#36365);
#8703=VERTEX_POINT('',#36367);
#8704=VERTEX_POINT('',#36376);
#8705=VERTEX_POINT('',#36378);
#8706=VERTEX_POINT('',#36385);
#8707=VERTEX_POINT('',#36443);
#8708=VERTEX_POINT('',#36444);
#8709=VERTEX_POINT('',#36451);
#8710=VERTEX_POINT('',#36453);
#8711=VERTEX_POINT('',#36517);
#8712=VERTEX_POINT('',#36519);
#8713=VERTEX_POINT('',#36591);
#8714=VERTEX_POINT('',#36598);
#8715=VERTEX_POINT('',#36662);
#8716=VERTEX_POINT('',#36663);
#8717=VERTEX_POINT('',#36665);
#8718=VERTEX_POINT('',#36667);
#8719=VERTEX_POINT('',#36736);
#8720=VERTEX_POINT('',#36737);
#8721=VERTEX_POINT('',#36810);
#8722=VERTEX_POINT('',#36817);
#8723=VERTEX_POINT('',#36881);
#8724=VERTEX_POINT('',#36882);
#8725=VERTEX_POINT('',#36884);
#8726=VERTEX_POINT('',#36886);
#8727=VERTEX_POINT('',#36956);
#8728=VERTEX_POINT('',#36957);
#8729=VERTEX_POINT('',#37030);
#8730=VERTEX_POINT('',#37032);
#8731=VERTEX_POINT('',#37096);
#8732=VERTEX_POINT('',#37097);
#8733=VERTEX_POINT('',#37099);
#8734=VERTEX_POINT('',#37101);
#8735=VERTEX_POINT('',#37165);
#8736=VERTEX_POINT('',#37167);
#8737=VERTEX_POINT('',#37239);
#8738=VERTEX_POINT('',#37246);
#8739=VERTEX_POINT('',#37264);
#8740=VERTEX_POINT('',#37266);
#8741=VERTEX_POINT('',#37269);
#8742=VERTEX_POINT('',#37271);
#8743=VERTEX_POINT('',#37274);
#8744=VERTEX_POINT('',#37276);
#8745=VERTEX_POINT('',#37281);
#8746=VERTEX_POINT('',#37282);
#8747=VERTEX_POINT('',#37284);
#8748=VERTEX_POINT('',#37286);
#8749=VERTEX_POINT('',#37288);
#8750=VERTEX_POINT('',#37290);
#8751=VERTEX_POINT('',#37294);
#8752=VERTEX_POINT('',#37295);
#8753=VERTEX_POINT('',#37297);
#8754=VERTEX_POINT('',#37299);
#8755=VERTEX_POINT('',#37301);
#8756=VERTEX_POINT('',#37303);
#8757=VERTEX_POINT('',#37315);
#8758=VERTEX_POINT('',#37316);
#8759=VERTEX_POINT('',#37324);
#8760=VERTEX_POINT('',#37328);
#8761=VERTEX_POINT('',#37332);
#8762=VERTEX_POINT('',#37339);
#8763=VERTEX_POINT('',#37343);
#8764=VERTEX_POINT('',#37347);
#8765=VERTEX_POINT('',#37354);
#8766=VERTEX_POINT('',#37358);
#8767=VERTEX_POINT('',#37362);
#8768=VERTEX_POINT('',#37371);
#8769=VERTEX_POINT('',#37378);
#8770=VERTEX_POINT('',#37382);
#8771=VERTEX_POINT('',#37386);
#8772=VERTEX_POINT('',#37393);
#8773=VERTEX_POINT('',#37397);
#8774=VERTEX_POINT('',#37401);
#8775=VERTEX_POINT('',#37408);
#8776=VERTEX_POINT('',#37412);
#8777=VERTEX_POINT('',#37416);
#8778=VERTEX_POINT('',#37423);
#8779=VERTEX_POINT('',#37429);
#8780=VERTEX_POINT('',#37431);
#8781=VERTEX_POINT('',#37435);
#8782=VERTEX_POINT('',#37439);
#8783=VERTEX_POINT('',#37443);
#8784=VERTEX_POINT('',#37447);
#8785=VERTEX_POINT('',#37453);
#8786=VERTEX_POINT('',#37455);
#8787=VERTEX_POINT('',#37459);
#8788=VERTEX_POINT('',#37463);
#8789=VERTEX_POINT('',#37467);
#8790=VERTEX_POINT('',#37471);
#8791=VERTEX_POINT('',#37477);
#8792=VERTEX_POINT('',#37478);
#8793=VERTEX_POINT('',#37480);
#8794=VERTEX_POINT('',#37482);
#8795=VERTEX_POINT('',#37486);
#8796=VERTEX_POINT('',#37487);
#8797=VERTEX_POINT('',#37489);
#8798=VERTEX_POINT('',#37491);
#8799=VERTEX_POINT('',#37495);
#8800=VERTEX_POINT('',#37496);
#8801=VERTEX_POINT('',#37498);
#8802=VERTEX_POINT('',#37500);
#8803=VERTEX_POINT('',#37504);
#8804=VERTEX_POINT('',#37505);
#8805=VERTEX_POINT('',#37507);
#8806=VERTEX_POINT('',#37509);
#8807=VERTEX_POINT('',#37514);
#8808=VERTEX_POINT('',#37516);
#8809=VERTEX_POINT('',#37520);
#8810=VERTEX_POINT('',#37521);
#8811=VERTEX_POINT('',#37523);
#8812=VERTEX_POINT('',#37525);
#8813=VERTEX_POINT('',#37529);
#8814=VERTEX_POINT('',#37530);
#8815=VERTEX_POINT('',#37532);
#8816=VERTEX_POINT('',#37534);
#8817=VERTEX_POINT('',#37538);
#8818=VERTEX_POINT('',#37539);
#8819=VERTEX_POINT('',#37541);
#8820=VERTEX_POINT('',#37543);
#8821=VERTEX_POINT('',#37552);
#8822=VERTEX_POINT('',#37554);
#8823=VERTEX_POINT('',#37559);
#8824=VERTEX_POINT('',#37560);
#8825=VERTEX_POINT('',#37567);
#8826=VERTEX_POINT('',#37569);
#8827=VERTEX_POINT('',#37573);
#8828=VERTEX_POINT('',#37575);
#8829=VERTEX_POINT('',#37579);
#8830=VERTEX_POINT('',#37581);
#8831=VERTEX_POINT('',#37583);
#8832=VERTEX_POINT('',#37585);
#8833=VERTEX_POINT('',#37587);
#8834=VERTEX_POINT('',#37589);
#8835=VERTEX_POINT('',#37593);
#8836=VERTEX_POINT('',#37594);
#8837=VERTEX_POINT('',#37596);
#8838=VERTEX_POINT('',#37598);
#8839=VERTEX_POINT('',#37602);
#8840=VERTEX_POINT('',#37604);
#8841=VERTEX_POINT('',#37606);
#8842=VERTEX_POINT('',#37613);
#8843=VERTEX_POINT('',#37614);
#8844=VERTEX_POINT('',#37616);
#8845=VERTEX_POINT('',#37621);
#8846=VERTEX_POINT('',#37625);
#8847=VERTEX_POINT('',#37626);
#8848=VERTEX_POINT('',#37629);
#8849=VERTEX_POINT('',#37633);
#8850=VERTEX_POINT('',#37635);
#8851=VERTEX_POINT('',#37639);
#8852=VERTEX_POINT('',#37640);
#8853=VERTEX_POINT('',#37645);
#8854=VERTEX_POINT('',#37647);
#8855=VERTEX_POINT('',#37651);
#8856=VERTEX_POINT('',#37652);
#8857=VERTEX_POINT('',#37654);
#8858=VERTEX_POINT('',#37656);
#8859=VERTEX_POINT('',#37660);
#8860=VERTEX_POINT('',#37662);
#8861=VERTEX_POINT('',#37669);
#8862=VERTEX_POINT('',#37671);
#8863=VERTEX_POINT('',#37675);
#8864=VERTEX_POINT('',#37677);
#8865=VERTEX_POINT('',#37679);
#8866=VERTEX_POINT('',#37681);
#8867=VERTEX_POINT('',#37683);
#8868=VERTEX_POINT('',#37685);
#8869=VERTEX_POINT('',#37689);
#8870=VERTEX_POINT('',#37690);
#8871=VERTEX_POINT('',#37692);
#8872=VERTEX_POINT('',#37694);
#8873=VERTEX_POINT('',#37698);
#8874=VERTEX_POINT('',#37700);
#8875=VERTEX_POINT('',#37707);
#8876=VERTEX_POINT('',#37708);
#8877=VERTEX_POINT('',#37710);
#8878=VERTEX_POINT('',#37712);
#8879=VERTEX_POINT('',#37717);
#8880=VERTEX_POINT('',#37721);
#8881=VERTEX_POINT('',#37725);
#8882=VERTEX_POINT('',#37727);
#8883=VERTEX_POINT('',#37729);
#8884=VERTEX_POINT('',#37731);
#8885=VERTEX_POINT('',#37733);
#8886=VERTEX_POINT('',#37735);
#8887=VERTEX_POINT('',#37739);
#8888=VERTEX_POINT('',#37740);
#8889=VERTEX_POINT('',#37742);
#8890=VERTEX_POINT('',#37744);
#8891=VERTEX_POINT('',#37746);
#8892=VERTEX_POINT('',#37748);
#8893=VERTEX_POINT('',#37752);
#8894=VERTEX_POINT('',#37753);
#8895=VERTEX_POINT('',#37755);
#8896=VERTEX_POINT('',#37757);
#8897=VERTEX_POINT('',#37762);
#8898=VERTEX_POINT('',#37763);
#8899=VERTEX_POINT('',#37766);
#8900=VERTEX_POINT('',#37768);
#8901=VERTEX_POINT('',#37772);
#8902=VERTEX_POINT('',#37774);
#8903=VERTEX_POINT('',#37778);
#8904=VERTEX_POINT('',#37780);
#8905=VERTEX_POINT('',#37784);
#8906=VERTEX_POINT('',#37788);
#8907=VERTEX_POINT('',#37792);
#8908=VERTEX_POINT('',#37796);
#8909=VERTEX_POINT('',#37800);
#8910=VERTEX_POINT('',#37804);
#8911=VERTEX_POINT('',#37806);
#8912=VERTEX_POINT('',#37810);
#8913=VERTEX_POINT('',#37812);
#8914=VERTEX_POINT('',#37814);
#8915=VERTEX_POINT('',#37818);
#8916=VERTEX_POINT('',#37820);
#8917=VERTEX_POINT('',#37824);
#8918=VERTEX_POINT('',#37826);
#8919=VERTEX_POINT('',#37830);
#8920=VERTEX_POINT('',#37834);
#8921=VERTEX_POINT('',#37838);
#8922=VERTEX_POINT('',#37842);
#8923=VERTEX_POINT('',#37846);
#8924=VERTEX_POINT('',#37850);
#8925=VERTEX_POINT('',#37852);
#8926=VERTEX_POINT('',#37856);
#8927=VERTEX_POINT('',#37858);
#8928=VERTEX_POINT('',#37860);
#8929=VERTEX_POINT('',#37864);
#8930=VERTEX_POINT('',#37866);
#8931=VERTEX_POINT('',#37870);
#8932=VERTEX_POINT('',#37872);
#8933=VERTEX_POINT('',#37876);
#8934=VERTEX_POINT('',#37880);
#8935=VERTEX_POINT('',#37884);
#8936=VERTEX_POINT('',#37888);
#8937=VERTEX_POINT('',#37892);
#8938=VERTEX_POINT('',#37896);
#8939=VERTEX_POINT('',#37898);
#8940=VERTEX_POINT('',#37902);
#8941=VERTEX_POINT('',#37904);
#8942=VERTEX_POINT('',#37906);
#8943=VERTEX_POINT('',#37910);
#8944=VERTEX_POINT('',#37912);
#8945=VERTEX_POINT('',#37916);
#8946=VERTEX_POINT('',#37918);
#8947=VERTEX_POINT('',#37922);
#8948=VERTEX_POINT('',#37926);
#8949=VERTEX_POINT('',#37930);
#8950=VERTEX_POINT('',#37934);
#8951=VERTEX_POINT('',#37938);
#8952=VERTEX_POINT('',#37942);
#8953=VERTEX_POINT('',#37946);
#8954=VERTEX_POINT('',#37948);
#8955=VERTEX_POINT('',#37952);
#8956=VERTEX_POINT('',#37956);
#8957=VERTEX_POINT('',#37960);
#8958=VERTEX_POINT('',#37964);
#8959=VERTEX_POINT('',#37984);
#8960=VERTEX_POINT('',#37986);
#8961=VERTEX_POINT('',#37990);
#8962=VERTEX_POINT('',#37991);
#8963=VERTEX_POINT('',#37993);
#8964=VERTEX_POINT('',#37995);
#8965=VERTEX_POINT('',#37998);
#8966=VERTEX_POINT('',#38002);
#8967=VERTEX_POINT('',#38006);
#8968=VERTEX_POINT('',#38010);
#8969=VERTEX_POINT('',#38014);
#8970=VERTEX_POINT('',#38016);
#8971=VERTEX_POINT('',#38018);
#8972=VERTEX_POINT('',#38029);
#8973=VERTEX_POINT('',#38031);
#8974=VERTEX_POINT('',#38033);
#8975=VERTEX_POINT('',#38035);
#8976=VERTEX_POINT('',#38039);
#8977=VERTEX_POINT('',#38043);
#8978=VERTEX_POINT('',#38047);
#8979=VERTEX_POINT('',#38051);
#8980=VERTEX_POINT('',#38053);
#8981=VERTEX_POINT('',#38055);
#8982=VERTEX_POINT('',#38057);
#8983=VERTEX_POINT('',#38059);
#8984=VERTEX_POINT('',#38063);
#8985=VERTEX_POINT('',#38070);
#8986=VERTEX_POINT('',#38071);
#8987=VERTEX_POINT('',#38073);
#8988=VERTEX_POINT('',#38075);
#8989=VERTEX_POINT('',#38077);
#8990=VERTEX_POINT('',#38079);
#8991=VERTEX_POINT('',#38112);
#8992=VERTEX_POINT('',#38113);
#8993=VERTEX_POINT('',#38115);
#8994=VERTEX_POINT('',#38117);
#8995=VERTEX_POINT('',#38119);
#8996=VERTEX_POINT('',#38121);
#8997=VERTEX_POINT('',#38123);
#8998=VERTEX_POINT('',#38125);
#8999=VERTEX_POINT('',#38132);
#9000=VERTEX_POINT('',#38134);
#9001=VERTEX_POINT('',#38138);
#9002=VERTEX_POINT('',#38139);
#9003=VERTEX_POINT('',#38141);
#9004=VERTEX_POINT('',#38143);
#9005=VERTEX_POINT('',#38145);
#9006=VERTEX_POINT('',#38147);
#9007=VERTEX_POINT('',#38152);
#9008=VERTEX_POINT('',#38153);
#9009=VERTEX_POINT('',#38155);
#9010=VERTEX_POINT('',#38157);
#9011=VERTEX_POINT('',#38159);
#9012=VERTEX_POINT('',#38161);
#9013=VERTEX_POINT('',#38176);
#9014=VERTEX_POINT('',#38178);
#9015=VERTEX_POINT('',#38182);
#9016=VERTEX_POINT('',#38186);
#9017=VERTEX_POINT('',#38190);
#9018=VERTEX_POINT('',#38194);
#9019=VERTEX_POINT('',#38200);
#9020=VERTEX_POINT('',#38202);
#9021=VERTEX_POINT('',#38214);
#9022=VERTEX_POINT('',#38215);
#9023=VERTEX_POINT('',#38222);
#9024=VERTEX_POINT('',#38223);
#9025=VERTEX_POINT('',#38225);
#9026=VERTEX_POINT('',#38227);
#9027=VERTEX_POINT('',#38229);
#9028=VERTEX_POINT('',#38231);
#9029=VERTEX_POINT('',#38235);
#9030=VERTEX_POINT('',#38236);
#9031=VERTEX_POINT('',#38238);
#9032=VERTEX_POINT('',#38240);
#9033=VERTEX_POINT('',#38242);
#9034=VERTEX_POINT('',#38244);
#9035=VERTEX_POINT('',#38248);
#9036=VERTEX_POINT('',#38249);
#9037=VERTEX_POINT('',#38251);
#9038=VERTEX_POINT('',#38253);
#9039=VERTEX_POINT('',#38255);
#9040=VERTEX_POINT('',#38257);
#9041=VERTEX_POINT('',#38261);
#9042=VERTEX_POINT('',#38265);
#9043=VERTEX_POINT('',#38271);
#9044=VERTEX_POINT('',#38275);
#9045=VERTEX_POINT('',#38284);
#9046=VERTEX_POINT('',#38288);
#9047=VERTEX_POINT('',#38294);
#9048=VERTEX_POINT('',#38298);
#9049=VERTEX_POINT('',#38304);
#9050=VERTEX_POINT('',#38306);
#9051=VERTEX_POINT('',#38310);
#9052=VERTEX_POINT('',#38314);
#9053=VERTEX_POINT('',#38318);
#9054=VERTEX_POINT('',#38322);
#9055=VERTEX_POINT('',#38328);
#9056=VERTEX_POINT('',#38330);
#9057=VERTEX_POINT('',#38334);
#9058=VERTEX_POINT('',#38343);
#9059=VERTEX_POINT('',#38345);
#9060=VERTEX_POINT('',#38349);
#9061=VERTEX_POINT('',#38358);
#9062=VERTEX_POINT('',#38362);
#9063=VERTEX_POINT('',#38363);
#9064=VERTEX_POINT('',#38365);
#9065=VERTEX_POINT('',#38367);
#9066=VERTEX_POINT('',#38369);
#9067=VERTEX_POINT('',#38371);
#9068=VERTEX_POINT('',#38375);
#9069=VERTEX_POINT('',#38376);
#9070=VERTEX_POINT('',#38378);
#9071=VERTEX_POINT('',#38380);
#9072=VERTEX_POINT('',#38382);
#9073=VERTEX_POINT('',#38384);
#9074=VERTEX_POINT('',#38388);
#9075=VERTEX_POINT('',#38389);
#9076=VERTEX_POINT('',#38391);
#9077=VERTEX_POINT('',#38393);
#9078=VERTEX_POINT('',#38395);
#9079=VERTEX_POINT('',#38397);
#9080=VERTEX_POINT('',#38401);
#9081=VERTEX_POINT('',#38405);
#9082=VERTEX_POINT('',#38411);
#9083=VERTEX_POINT('',#38412);
#9084=VERTEX_POINT('',#38414);
#9085=VERTEX_POINT('',#38416);
#9086=VERTEX_POINT('',#38418);
#9087=VERTEX_POINT('',#38420);
#9088=VERTEX_POINT('',#38424);
#9089=VERTEX_POINT('',#38425);
#9090=VERTEX_POINT('',#38427);
#9091=VERTEX_POINT('',#38429);
#9092=VERTEX_POINT('',#38431);
#9093=VERTEX_POINT('',#38433);
#9094=VERTEX_POINT('',#38437);
#9095=VERTEX_POINT('',#38439);
#9096=VERTEX_POINT('',#38443);
#9097=VERTEX_POINT('',#38447);
#9098=VERTEX_POINT('',#38451);
#9099=VERTEX_POINT('',#38455);
#9100=VERTEX_POINT('',#38461);
#9101=VERTEX_POINT('',#38462);
#9102=VERTEX_POINT('',#38464);
#9103=VERTEX_POINT('',#38468);
#9104=VERTEX_POINT('',#38469);
#9105=VERTEX_POINT('',#38474);
#9106=VERTEX_POINT('',#38476);
#9107=VERTEX_POINT('',#38478);
#9108=VERTEX_POINT('',#38482);
#9109=VERTEX_POINT('',#38484);
#9110=VERTEX_POINT('',#38488);
#9111=VERTEX_POINT('',#38492);
#9112=VERTEX_POINT('',#38496);
#9113=VERTEX_POINT('',#38500);
#9114=VERTEX_POINT('',#38506);
#9115=VERTEX_POINT('',#38507);
#9116=VERTEX_POINT('',#38509);
#9117=VERTEX_POINT('',#38511);
#9118=VERTEX_POINT('',#38515);
#9119=VERTEX_POINT('',#38517);
#9120=VERTEX_POINT('',#38519);
#9121=VERTEX_POINT('',#38523);
#9122=VERTEX_POINT('',#38525);
#9123=VERTEX_POINT('',#38529);
#9124=VERTEX_POINT('',#38533);
#9125=VERTEX_POINT('',#38537);
#9126=VERTEX_POINT('',#38541);
#9127=VERTEX_POINT('',#38547);
#9128=VERTEX_POINT('',#38548);
#9129=VERTEX_POINT('',#38563);
#9130=VERTEX_POINT('',#38576);
#9131=VERTEX_POINT('',#38590);
#9132=VERTEX_POINT('',#38601);
#9133=VERTEX_POINT('',#38603);
#9134=VERTEX_POINT('',#38615);
#9135=VERTEX_POINT('',#38616);
#9136=VERTEX_POINT('',#38621);
#9137=VERTEX_POINT('',#38630);
#9138=VERTEX_POINT('',#38631);
#9139=VERTEX_POINT('',#38636);
#9140=VERTEX_POINT('',#38647);
#9141=VERTEX_POINT('',#38660);
#9142=VERTEX_POINT('',#38674);
#9143=VERTEX_POINT('',#38687);
#9144=VERTEX_POINT('',#38701);
#9145=VERTEX_POINT('',#38708);
#9146=VERTEX_POINT('',#38721);
#9147=VERTEX_POINT('',#38742);
#9148=VERTEX_POINT('',#38743);
#9149=VERTEX_POINT('',#38787);
#9150=VERTEX_POINT('',#38844);
#9151=VERTEX_POINT('',#38845);
#9152=VERTEX_POINT('',#38847);
#9153=VERTEX_POINT('',#38849);
#9154=VERTEX_POINT('',#38851);
#9155=VERTEX_POINT('',#38854);
#9156=VERTEX_POINT('',#38858);
#9157=VERTEX_POINT('',#38859);
#9158=VERTEX_POINT('',#38864);
#9159=VERTEX_POINT('',#38868);
#9160=VERTEX_POINT('',#38870);
#9161=VERTEX_POINT('',#38874);
#9162=VERTEX_POINT('',#38876);
#9163=VERTEX_POINT('',#38881);
#9164=VERTEX_POINT('',#38883);
#9165=VERTEX_POINT('',#38887);
#9166=VERTEX_POINT('',#38891);
#9167=VERTEX_POINT('',#38895);
#9168=VERTEX_POINT('',#38899);
#9169=VERTEX_POINT('',#38922);
#9170=VERTEX_POINT('',#38979);
#9171=VERTEX_POINT('',#38981);
#9172=VERTEX_POINT('',#38985);
#9173=VERTEX_POINT('',#38989);
#9174=VERTEX_POINT('',#38991);
#9175=VERTEX_POINT('',#38995);
#9176=VERTEX_POINT('',#38997);
#9177=VERTEX_POINT('',#39001);
#9178=VERTEX_POINT('',#39005);
#9179=VERTEX_POINT('',#39009);
#9180=VERTEX_POINT('',#39013);
#9181=VERTEX_POINT('',#39019);
#9182=VERTEX_POINT('',#39021);
#9183=VERTEX_POINT('',#39025);
#9184=VERTEX_POINT('',#39029);
#9185=VERTEX_POINT('',#39033);
#9186=VERTEX_POINT('',#39037);
#9187=VERTEX_POINT('',#39044);
#9188=VERTEX_POINT('',#39045);
#9189=VERTEX_POINT('',#39047);
#9190=VERTEX_POINT('',#39049);
#9191=VERTEX_POINT('',#39051);
#9192=VERTEX_POINT('',#39053);
#9193=VERTEX_POINT('',#39058);
#9194=VERTEX_POINT('',#39059);
#9195=VERTEX_POINT('',#39061);
#9196=VERTEX_POINT('',#39063);
#9197=VERTEX_POINT('',#39065);
#9198=VERTEX_POINT('',#39067);
#9199=VERTEX_POINT('',#39071);
#9200=VERTEX_POINT('',#39072);
#9201=VERTEX_POINT('',#39077);
#9202=VERTEX_POINT('',#39079);
#9203=VERTEX_POINT('',#39081);
#9204=VERTEX_POINT('',#39083);
#9205=VERTEX_POINT('',#39087);
#9206=VERTEX_POINT('',#39088);
#9207=VERTEX_POINT('',#39093);
#9208=VERTEX_POINT('',#39095);
#9209=VERTEX_POINT('',#39099);
#9210=VERTEX_POINT('',#39103);
#9211=VERTEX_POINT('',#39107);
#9212=VERTEX_POINT('',#39111);
#9213=VERTEX_POINT('',#39117);
#9214=VERTEX_POINT('',#39118);
#9215=VERTEX_POINT('',#39120);
#9216=VERTEX_POINT('',#39123);
#9217=VERTEX_POINT('',#39127);
#9218=VERTEX_POINT('',#39131);
#9219=VERTEX_POINT('',#39135);
#9220=VERTEX_POINT('',#39137);
#9221=VERTEX_POINT('',#39139);
#9222=VERTEX_POINT('',#39143);
#9223=VERTEX_POINT('',#39152);
#9224=VERTEX_POINT('',#39173);
#9225=VERTEX_POINT('',#39174);
#9226=VERTEX_POINT('',#39181);
#9227=VERTEX_POINT('',#39234);
#9228=VERTEX_POINT('',#39238);
#9229=VERTEX_POINT('',#39240);
#9230=VERTEX_POINT('',#39261);
#9231=VERTEX_POINT('',#39318);
#9232=VERTEX_POINT('',#39320);
#9233=VERTEX_POINT('',#39324);
#9234=VERTEX_POINT('',#39325);
#9235=VERTEX_POINT('',#39330);
#9236=VERTEX_POINT('',#39336);
#9237=VERTEX_POINT('',#39340);
#9238=VERTEX_POINT('',#39344);
#9239=VERTEX_POINT('',#39349);
#9240=VERTEX_POINT('',#39351);
#9241=VERTEX_POINT('',#39355);
#9242=VERTEX_POINT('',#39359);
#9243=VERTEX_POINT('',#39363);
#9244=VERTEX_POINT('',#39367);
#9245=VERTEX_POINT('',#39377);
#9246=VERTEX_POINT('',#39378);
#9247=VERTEX_POINT('',#39383);
#9248=VERTEX_POINT('',#39387);
#9249=VERTEX_POINT('',#39401);
#9250=VERTEX_POINT('',#39402);
#9251=VERTEX_POINT('',#39406);
#9252=VERTEX_POINT('',#39407);
#9253=VERTEX_POINT('',#39413);
#9254=VERTEX_POINT('',#39417);
#9255=VERTEX_POINT('',#39418);
#9256=VERTEX_POINT('',#39423);
#9257=VERTEX_POINT('',#39427);
#9258=VERTEX_POINT('',#39428);
#9259=VERTEX_POINT('',#39438);
#9260=VERTEX_POINT('',#39439);
#9261=VERTEX_POINT('',#39443);
#9262=VERTEX_POINT('',#39444);
#9263=VERTEX_POINT('',#39448);
#9264=VERTEX_POINT('',#39452);
#9265=VERTEX_POINT('',#39454);
#9266=VERTEX_POINT('',#39465);
#9267=VERTEX_POINT('',#39467);
#9268=VERTEX_POINT('',#39469);
#9269=VERTEX_POINT('',#39471);
#9270=VERTEX_POINT('',#39487);
#9271=VERTEX_POINT('',#39488);
#9272=VERTEX_POINT('',#39491);
#9273=VERTEX_POINT('',#39493);
#9274=VERTEX_POINT('',#39495);
#9275=VERTEX_POINT('',#39499);
#9276=VERTEX_POINT('',#39503);
#9277=VERTEX_POINT('',#39505);
#9278=VERTEX_POINT('',#39509);
#9279=VERTEX_POINT('',#39513);
#9280=VERTEX_POINT('',#39515);
#9281=VERTEX_POINT('',#39519);
#9282=VERTEX_POINT('',#39523);
#9283=VERTEX_POINT('',#39524);
#9284=VERTEX_POINT('',#39526);
#9285=VERTEX_POINT('',#39528);
#9286=VERTEX_POINT('',#39530);
#9287=VERTEX_POINT('',#39532);
#9288=VERTEX_POINT('',#39535);
#9289=VERTEX_POINT('',#39537);
#9290=VERTEX_POINT('',#39539);
#9291=VERTEX_POINT('',#39543);
#9292=VERTEX_POINT('',#39547);
#9293=VERTEX_POINT('',#39548);
#9294=VERTEX_POINT('',#39553);
#9295=VERTEX_POINT('',#39557);
#9296=VERTEX_POINT('',#39558);
#9297=VERTEX_POINT('',#39563);
#9298=VERTEX_POINT('',#39567);
#9299=VERTEX_POINT('',#39568);
#9300=VERTEX_POINT('',#39571);
#9301=VERTEX_POINT('',#39573);
#9302=VERTEX_POINT('',#39577);
#9303=VERTEX_POINT('',#39578);
#9304=VERTEX_POINT('',#39583);
#9305=VERTEX_POINT('',#39588);
#9306=VERTEX_POINT('',#39589);
#9307=VERTEX_POINT('',#39594);
#9308=VERTEX_POINT('',#39595);
#9309=VERTEX_POINT('',#39600);
#9310=VERTEX_POINT('',#39604);
#9311=VERTEX_POINT('',#39609);
#9312=VERTEX_POINT('',#39617);
#9313=VERTEX_POINT('',#39621);
#9314=VERTEX_POINT('',#39626);
#9315=VERTEX_POINT('',#39629);
#9316=VERTEX_POINT('',#39635);
#9317=VERTEX_POINT('',#39642);
#9318=VERTEX_POINT('',#39649);
#9319=VERTEX_POINT('',#39658);
#9320=VERTEX_POINT('',#39659);
#9321=VERTEX_POINT('',#39661);
#9322=VERTEX_POINT('',#39666);
#9323=VERTEX_POINT('',#39668);
#9324=VERTEX_POINT('',#39672);
#9325=VERTEX_POINT('',#39683);
#9326=VERTEX_POINT('',#39684);
#9327=VERTEX_POINT('',#39689);
#9328=VERTEX_POINT('',#39693);
#9329=VERTEX_POINT('',#39697);
#9330=VERTEX_POINT('',#39699);
#9331=VERTEX_POINT('',#39703);
#9332=VERTEX_POINT('',#39704);
#9333=VERTEX_POINT('',#39709);
#9334=VERTEX_POINT('',#39713);
#9335=VERTEX_POINT('',#39723);
#9336=VERTEX_POINT('',#39724);
#9337=VERTEX_POINT('',#39727);
#9338=VERTEX_POINT('',#39731);
#9339=VERTEX_POINT('',#39735);
#9340=VERTEX_POINT('',#39737);
#9341=VERTEX_POINT('',#39741);
#9342=VERTEX_POINT('',#39743);
#9343=VERTEX_POINT('',#39747);
#9344=VERTEX_POINT('',#39751);
#9345=VERTEX_POINT('',#39755);
#9346=VERTEX_POINT('',#39759);
#9347=VERTEX_POINT('',#39763);
#9348=VERTEX_POINT('',#39767);
#9349=VERTEX_POINT('',#39771);
#9350=VERTEX_POINT('',#39775);
#9351=VERTEX_POINT('',#39779);
#9352=VERTEX_POINT('',#39783);
#9353=VERTEX_POINT('',#39791);
#9354=VERTEX_POINT('',#39792);
#9355=VERTEX_POINT('',#39795);
#9356=VERTEX_POINT('',#39799);
#9357=VERTEX_POINT('',#39800);
#9358=VERTEX_POINT('',#39802);
#9359=VERTEX_POINT('',#39804);
#9360=VERTEX_POINT('',#39806);
#9361=VERTEX_POINT('',#39809);
#9362=VERTEX_POINT('',#39811);
#9363=VERTEX_POINT('',#39815);
#9364=VERTEX_POINT('',#39817);
#9365=VERTEX_POINT('',#39825);
#9366=VERTEX_POINT('',#39829);
#9367=VERTEX_POINT('',#39833);
#9368=VERTEX_POINT('',#39837);
#9369=VERTEX_POINT('',#39841);
#9370=VERTEX_POINT('',#39845);
#9371=VERTEX_POINT('',#39849);
#9372=VERTEX_POINT('',#39850);
#9373=VERTEX_POINT('',#39852);
#9374=VERTEX_POINT('',#39854);
#9375=VERTEX_POINT('',#39856);
#9376=VERTEX_POINT('',#39858);
#9377=VERTEX_POINT('',#39862);
#9378=VERTEX_POINT('',#39870);
#9379=VERTEX_POINT('',#39878);
#9380=VERTEX_POINT('',#39886);
#9381=VERTEX_POINT('',#39894);
#9382=VERTEX_POINT('',#39902);
#9383=EDGE_CURVE('',#7676,#7676,#6997,.T.);
#9384=EDGE_CURVE('',#7676,#7677,#6998,.T.);
#9385=EDGE_CURVE('',#7677,#7677,#6999,.T.);
#9386=EDGE_CURVE('',#7678,#7679,#7000,.T.);
#9387=EDGE_CURVE('',#7679,#7678,#7001,.T.);
#9388=EDGE_CURVE('',#7679,#7680,#7002,.T.);
#9389=EDGE_CURVE('',#7680,#7680,#7003,.T.);
#9390=EDGE_CURVE('',#7681,#7682,#7004,.T.);
#9391=EDGE_CURVE('',#7682,#7683,#1408,.T.);
#9392=EDGE_CURVE('',#7684,#7683,#1368,.T.);
#9393=EDGE_CURVE('',#7685,#7684,#1409,.T.);
#9394=EDGE_CURVE('',#7685,#7686,#7005,.T.);
#9395=EDGE_CURVE('',#7686,#7687,#1410,.T.);
#9396=EDGE_CURVE('',#7688,#7687,#1369,.T.);
#9397=EDGE_CURVE('',#7689,#7688,#1411,.T.);
#9398=EDGE_CURVE('',#7689,#7690,#7006,.T.);
#9399=EDGE_CURVE('',#7690,#7691,#1412,.T.);
#9400=EDGE_CURVE('',#7692,#7691,#1370,.T.);
#9401=EDGE_CURVE('',#7693,#7692,#1413,.T.);
#9402=EDGE_CURVE('',#7693,#7694,#7007,.T.);
#9403=EDGE_CURVE('',#7694,#7695,#1414,.T.);
#9404=EDGE_CURVE('',#7696,#7695,#1371,.T.);
#9405=EDGE_CURVE('',#7697,#7696,#1415,.T.);
#9406=EDGE_CURVE('',#7697,#7698,#7008,.T.);
#9407=EDGE_CURVE('',#7698,#7699,#1416,.T.);
#9408=EDGE_CURVE('',#7699,#7699,#7009,.T.);
#9409=EDGE_CURVE('',#7698,#7700,#7010,.T.);
#9410=EDGE_CURVE('',#7700,#7701,#1417,.T.);
#9411=EDGE_CURVE('',#7702,#7701,#1372,.T.);
#9412=EDGE_CURVE('',#7703,#7702,#1418,.T.);
#9413=EDGE_CURVE('',#7703,#7704,#7011,.T.);
#9414=EDGE_CURVE('',#7704,#7705,#1419,.T.);
#9415=EDGE_CURVE('',#7706,#7705,#1373,.T.);
#9416=EDGE_CURVE('',#7707,#7706,#1420,.T.);
#9417=EDGE_CURVE('',#7707,#7708,#7012,.T.);
#9418=EDGE_CURVE('',#7708,#7709,#1421,.T.);
#9419=EDGE_CURVE('',#7710,#7709,#1374,.T.);
#9420=EDGE_CURVE('',#7711,#7710,#1422,.T.);
#9421=EDGE_CURVE('',#7711,#7712,#7013,.T.);
#9422=EDGE_CURVE('',#7712,#7713,#1423,.T.);
#9423=EDGE_CURVE('',#7714,#7713,#1375,.T.);
#9424=EDGE_CURVE('',#7715,#7714,#1424,.T.);
#9425=EDGE_CURVE('',#7715,#7716,#7014,.T.);
#9426=EDGE_CURVE('',#7716,#7717,#1425,.T.);
#9427=EDGE_CURVE('',#7718,#7717,#1376,.T.);
#9428=EDGE_CURVE('',#7681,#7718,#1426,.T.);
#9429=EDGE_CURVE('',#7719,#7719,#7015,.T.);
#9430=EDGE_CURVE('',#7719,#7720,#1427,.T.);
#9431=EDGE_CURVE('',#7720,#7720,#7016,.T.);
#9432=EDGE_CURVE('',#7721,#7721,#7017,.T.);
#9433=EDGE_CURVE('',#7721,#7722,#1428,.T.);
#9434=EDGE_CURVE('',#7722,#7722,#7018,.T.);
#9435=EDGE_CURVE('',#7723,#7723,#7019,.T.);
#9436=EDGE_CURVE('',#7723,#7724,#1429,.T.);
#9437=EDGE_CURVE('',#7724,#7724,#7020,.T.);
#9438=EDGE_CURVE('',#7725,#7725,#7021,.T.);
#9439=EDGE_CURVE('',#7725,#7726,#1430,.T.);
#9440=EDGE_CURVE('',#7726,#7726,#7022,.T.);
#9441=EDGE_CURVE('',#7727,#7727,#7023,.T.);
#9442=EDGE_CURVE('',#7727,#7728,#1431,.T.);
#9443=EDGE_CURVE('',#7728,#7728,#7024,.T.);
#9444=EDGE_CURVE('',#7729,#7729,#7025,.T.);
#9445=EDGE_CURVE('',#7729,#7730,#1432,.T.);
#9446=EDGE_CURVE('',#7730,#7730,#7026,.T.);
#9447=EDGE_CURVE('',#7731,#7731,#7027,.T.);
#9448=EDGE_CURVE('',#7731,#7732,#1433,.T.);
#9449=EDGE_CURVE('',#7732,#7732,#7028,.T.);
#9450=EDGE_CURVE('',#7733,#7733,#7029,.T.);
#9451=EDGE_CURVE('',#7733,#7734,#1434,.T.);
#9452=EDGE_CURVE('',#7734,#7734,#7030,.T.);
#9453=EDGE_CURVE('',#7735,#7735,#1065,.T.);
#9454=EDGE_CURVE('',#7735,#7736,#1435,.T.);
#9455=EDGE_CURVE('',#7736,#7736,#7031,.T.);
#9456=EDGE_CURVE('',#7737,#7737,#1066,.T.);
#9457=EDGE_CURVE('',#7737,#7738,#1436,.T.);
#9458=EDGE_CURVE('',#7738,#7738,#7032,.T.);
#9459=EDGE_CURVE('',#7739,#7739,#1067,.T.);
#9460=EDGE_CURVE('',#7739,#7740,#1437,.T.);
#9461=EDGE_CURVE('',#7740,#7740,#7033,.T.);
#9462=EDGE_CURVE('',#7741,#7741,#1068,.T.);
#9463=EDGE_CURVE('',#7741,#7742,#1438,.T.);
#9464=EDGE_CURVE('',#7742,#7742,#7034,.T.);
#9465=EDGE_CURVE('',#7677,#7743,#1439,.T.);
#9466=EDGE_CURVE('',#7743,#7743,#7035,.T.);
#9467=EDGE_CURVE('',#7744,#7744,#7036,.T.);
#9468=EDGE_CURVE('',#7744,#7745,#1440,.T.);
#9469=EDGE_CURVE('',#7745,#7745,#7037,.T.);
#9470=EDGE_CURVE('',#7746,#7746,#7038,.T.);
#9471=EDGE_CURVE('',#7746,#7747,#1441,.T.);
#9472=EDGE_CURVE('',#7747,#7747,#7039,.T.);
#9473=EDGE_CURVE('',#7748,#7748,#7040,.T.);
#9474=EDGE_CURVE('',#7748,#7749,#1442,.T.);
#9475=EDGE_CURVE('',#7749,#7749,#7041,.T.);
#9476=EDGE_CURVE('',#7750,#7750,#7042,.T.);
#9477=EDGE_CURVE('',#7750,#7751,#1443,.T.);
#9478=EDGE_CURVE('',#7751,#7751,#7043,.T.);
#9479=EDGE_CURVE('',#7752,#7752,#7044,.T.);
#9480=EDGE_CURVE('',#7752,#7753,#1444,.T.);
#9481=EDGE_CURVE('',#7753,#7753,#7045,.T.);
#9482=EDGE_CURVE('',#7754,#7754,#7046,.T.);
#9483=EDGE_CURVE('',#7754,#7755,#1445,.T.);
#9484=EDGE_CURVE('',#7755,#7755,#7047,.T.);
#9485=EDGE_CURVE('',#7756,#7756,#7048,.T.);
#9486=EDGE_CURVE('',#7756,#7757,#1446,.T.);
#9487=EDGE_CURVE('',#7757,#7757,#7049,.T.);
#9488=EDGE_CURVE('',#7758,#7758,#7050,.T.);
#9489=EDGE_CURVE('',#7758,#7759,#1447,.T.);
#9490=EDGE_CURVE('',#7759,#7759,#7051,.T.);
#9491=EDGE_CURVE('',#7760,#7760,#7052,.T.);
#9492=EDGE_CURVE('',#7760,#7761,#1448,.T.);
#9493=EDGE_CURVE('',#7761,#7761,#7053,.T.);
#9494=EDGE_CURVE('',#7762,#7762,#7054,.T.);
#9495=EDGE_CURVE('',#7762,#7763,#1449,.T.);
#9496=EDGE_CURVE('',#7763,#7763,#7055,.T.);
#9497=EDGE_CURVE('',#7764,#7764,#7056,.T.);
#9498=EDGE_CURVE('',#7764,#7765,#1450,.T.);
#9499=EDGE_CURVE('',#7765,#7765,#7057,.T.);
#9500=EDGE_CURVE('',#7766,#7766,#7058,.T.);
#9501=EDGE_CURVE('',#7766,#7767,#1451,.T.);
#9502=EDGE_CURVE('',#7767,#7767,#7059,.T.);
#9503=EDGE_CURVE('',#7768,#7768,#7060,.T.);
#9504=EDGE_CURVE('',#7768,#7769,#1452,.T.);
#9505=EDGE_CURVE('',#7769,#7769,#7061,.T.);
#9506=EDGE_CURVE('',#7770,#7770,#7062,.T.);
#9507=EDGE_CURVE('',#7770,#7771,#1453,.T.);
#9508=EDGE_CURVE('',#7771,#7771,#7063,.T.);
#9509=EDGE_CURVE('',#7772,#7772,#7064,.T.);
#9510=EDGE_CURVE('',#7772,#7773,#1454,.T.);
#9511=EDGE_CURVE('',#7773,#7773,#7065,.T.);
#9512=EDGE_CURVE('',#7678,#7774,#1455,.T.);
#9513=EDGE_CURVE('',#7774,#7774,#7066,.T.);
#9514=EDGE_CURVE('',#7775,#7775,#7067,.T.);
#9515=EDGE_CURVE('',#7775,#7776,#1456,.T.);
#9516=EDGE_CURVE('',#7776,#7776,#7068,.T.);
#9517=EDGE_CURVE('',#7777,#7777,#7069,.T.);
#9518=EDGE_CURVE('',#7777,#7778,#1457,.T.);
#9519=EDGE_CURVE('',#7778,#7778,#7070,.T.);
#9520=EDGE_CURVE('',#7704,#7779,#1458,.T.);
#9521=EDGE_CURVE('',#7703,#7780,#1459,.T.);
#9522=EDGE_CURVE('',#7781,#7780,#1460,.T.);
#9523=EDGE_CURVE('',#7700,#7781,#1461,.T.);
#9524=EDGE_CURVE('',#7697,#7782,#1462,.T.);
#9525=EDGE_CURVE('',#7783,#7782,#1463,.T.);
#9526=EDGE_CURVE('',#7694,#7783,#1464,.T.);
#9527=EDGE_CURVE('',#7693,#7784,#1465,.T.);
#9528=EDGE_CURVE('',#7785,#7784,#1466,.T.);
#9529=EDGE_CURVE('',#7690,#7785,#1467,.T.);
#9530=EDGE_CURVE('',#7689,#7786,#1468,.T.);
#9531=EDGE_CURVE('',#7787,#7786,#1469,.T.);
#9532=EDGE_CURVE('',#7686,#7787,#1470,.T.);
#9533=EDGE_CURVE('',#7685,#7788,#1471,.T.);
#9534=EDGE_CURVE('',#7789,#7788,#1472,.T.);
#9535=EDGE_CURVE('',#7682,#7789,#1473,.T.);
#9536=EDGE_CURVE('',#7681,#7790,#1474,.T.);
#9537=EDGE_CURVE('',#7791,#7790,#1475,.T.);
#9538=EDGE_CURVE('',#7716,#7791,#1476,.T.);
#9539=EDGE_CURVE('',#7715,#7792,#1477,.T.);
#9540=EDGE_CURVE('',#7793,#7792,#1478,.T.);
#9541=EDGE_CURVE('',#7712,#7793,#1479,.T.);
#9542=EDGE_CURVE('',#7711,#7794,#1480,.T.);
#9543=EDGE_CURVE('',#7795,#7794,#1481,.T.);
#9544=EDGE_CURVE('',#7708,#7795,#1482,.T.);
#9545=EDGE_CURVE('',#7707,#7796,#1483,.T.);
#9546=EDGE_CURVE('',#7779,#7796,#1484,.T.);
#9547=EDGE_CURVE('',#7797,#7798,#7071,.T.);
#9548=EDGE_CURVE('',#7798,#7799,#1485,.T.);
#9549=EDGE_CURVE('',#7799,#7800,#7072,.T.);
#9550=EDGE_CURVE('',#7800,#7801,#1486,.T.);
#9551=EDGE_CURVE('',#7801,#7802,#7073,.T.);
#9552=EDGE_CURVE('',#7802,#7803,#1487,.T.);
#9553=EDGE_CURVE('',#7803,#7804,#7074,.T.);
#9554=EDGE_CURVE('',#7804,#7797,#1488,.T.);
#9555=EDGE_CURVE('',#7805,#7806,#7075,.T.);
#9556=EDGE_CURVE('',#7807,#7805,#1489,.T.);
#9557=EDGE_CURVE('',#7808,#7807,#7076,.T.);
#9558=EDGE_CURVE('',#7809,#7808,#1490,.T.);
#9559=EDGE_CURVE('',#7810,#7809,#7077,.T.);
#9560=EDGE_CURVE('',#7811,#7810,#1491,.T.);
#9561=EDGE_CURVE('',#7812,#7811,#7078,.T.);
#9562=EDGE_CURVE('',#7806,#7812,#1492,.T.);
#9563=EDGE_CURVE('',#7798,#7806,#1493,.T.);
#9564=EDGE_CURVE('',#7797,#7805,#1494,.T.);
#9565=EDGE_CURVE('',#7799,#7812,#1495,.T.);
#9566=EDGE_CURVE('',#7800,#7811,#1496,.T.);
#9567=EDGE_CURVE('',#7801,#7810,#1497,.T.);
#9568=EDGE_CURVE('',#7802,#7809,#1498,.T.);
#9569=EDGE_CURVE('',#7803,#7808,#1499,.T.);
#9570=EDGE_CURVE('',#7804,#7807,#1500,.T.);
#9571=EDGE_CURVE('',#7813,#7814,#7079,.T.);
#9572=EDGE_CURVE('',#7814,#7815,#1501,.T.);
#9573=EDGE_CURVE('',#7815,#7816,#7080,.T.);
#9574=EDGE_CURVE('',#7816,#7817,#1502,.T.);
#9575=EDGE_CURVE('',#7817,#7818,#7081,.T.);
#9576=EDGE_CURVE('',#7818,#7819,#1503,.T.);
#9577=EDGE_CURVE('',#7819,#7820,#7082,.T.);
#9578=EDGE_CURVE('',#7820,#7813,#1504,.T.);
#9579=EDGE_CURVE('',#7821,#7822,#7083,.T.);
#9580=EDGE_CURVE('',#7823,#7821,#1505,.T.);
#9581=EDGE_CURVE('',#7824,#7823,#7084,.T.);
#9582=EDGE_CURVE('',#7825,#7824,#1506,.T.);
#9583=EDGE_CURVE('',#7826,#7825,#7085,.T.);
#9584=EDGE_CURVE('',#7827,#7826,#1507,.T.);
#9585=EDGE_CURVE('',#7828,#7827,#7086,.T.);
#9586=EDGE_CURVE('',#7822,#7828,#1508,.T.);
#9587=EDGE_CURVE('',#7814,#7822,#1509,.T.);
#9588=EDGE_CURVE('',#7813,#7821,#1510,.T.);
#9589=EDGE_CURVE('',#7815,#7828,#1511,.T.);
#9590=EDGE_CURVE('',#7816,#7827,#1512,.T.);
#9591=EDGE_CURVE('',#7817,#7826,#1513,.T.);
#9592=EDGE_CURVE('',#7818,#7825,#1514,.T.);
#9593=EDGE_CURVE('',#7819,#7824,#1515,.T.);
#9594=EDGE_CURVE('',#7820,#7823,#1516,.T.);
#9595=EDGE_CURVE('',#7795,#7709,#1517,.T.);
#9596=EDGE_CURVE('',#7794,#7710,#1518,.T.);
#9597=EDGE_CURVE('',#7793,#7713,#1519,.T.);
#9598=EDGE_CURVE('',#7792,#7714,#1520,.T.);
#9599=EDGE_CURVE('',#7791,#7717,#1521,.T.);
#9600=EDGE_CURVE('',#7790,#7718,#1522,.T.);
#9601=EDGE_CURVE('',#7789,#7683,#1523,.T.);
#9602=EDGE_CURVE('',#7788,#7684,#1524,.T.);
#9603=EDGE_CURVE('',#7787,#7687,#1525,.T.);
#9604=EDGE_CURVE('',#7786,#7688,#1526,.T.);
#9605=EDGE_CURVE('',#7785,#7691,#1527,.T.);
#9606=EDGE_CURVE('',#7784,#7692,#1528,.T.);
#9607=EDGE_CURVE('',#7783,#7695,#1529,.T.);
#9608=EDGE_CURVE('',#7782,#7696,#1530,.T.);
#9609=EDGE_CURVE('',#7781,#7701,#1531,.T.);
#9610=EDGE_CURVE('',#7780,#7702,#1532,.T.);
#9611=EDGE_CURVE('',#7779,#7705,#1533,.T.);
#9612=EDGE_CURVE('',#7796,#7706,#1534,.T.);
#9613=EDGE_CURVE('',#7829,#7830,#7087,.T.);
#9614=EDGE_CURVE('',#7830,#7831,#1535,.T.);
#9615=EDGE_CURVE('',#7832,#7831,#7088,.T.);
#9616=EDGE_CURVE('',#7829,#7832,#1536,.T.);
#9617=EDGE_CURVE('',#7830,#7829,#7089,.T.);
#9618=EDGE_CURVE('',#7831,#7832,#7090,.T.);
#9619=EDGE_CURVE('',#7833,#7833,#7091,.T.);
#9620=EDGE_CURVE('',#7833,#7834,#1537,.T.);
#9621=EDGE_CURVE('',#7835,#7834,#1069,.T.);
#9622=EDGE_CURVE('',#7836,#7835,#1070,.T.);
#9623=EDGE_CURVE('',#7837,#7836,#1071,.T.);
#9624=EDGE_CURVE('',#7838,#7837,#1072,.T.);
#9625=EDGE_CURVE('',#7839,#7838,#1073,.T.);
#9626=EDGE_CURVE('',#7840,#7839,#1074,.T.);
#9627=EDGE_CURVE('',#7841,#7840,#1075,.T.);
#9628=EDGE_CURVE('',#7834,#7841,#1076,.T.);
#9629=EDGE_CURVE('',#7842,#7843,#7092,.T.);
#9630=EDGE_CURVE('',#7844,#7842,#1538,.T.);
#9631=EDGE_CURVE('',#7844,#7845,#7093,.T.);
#9632=EDGE_CURVE('',#7843,#7845,#1539,.T.);
#9633=EDGE_CURVE('',#7845,#7844,#7094,.T.);
#9634=EDGE_CURVE('',#7842,#7843,#7095,.T.);
#9635=EDGE_CURVE('',#7846,#7847,#7096,.T.);
#9636=EDGE_CURVE('',#7847,#7846,#7097,.T.);
#9637=EDGE_CURVE('',#7848,#7847,#1540,.T.);
#9638=EDGE_CURVE('',#7849,#7848,#7098,.T.);
#9639=EDGE_CURVE('',#7849,#7846,#1541,.T.);
#9640=EDGE_CURVE('',#7848,#7849,#7099,.T.);
#9641=EDGE_CURVE('',#7835,#7836,#1077,.T.);
#9642=EDGE_CURVE('',#7834,#7835,#1078,.T.);
#9643=EDGE_CURVE('',#7841,#7834,#1079,.T.);
#9644=EDGE_CURVE('',#7840,#7841,#1080,.T.);
#9645=EDGE_CURVE('',#7839,#7840,#1081,.T.);
#9646=EDGE_CURVE('',#7838,#7839,#1082,.T.);
#9647=EDGE_CURVE('',#7837,#7838,#1083,.T.);
#9648=EDGE_CURVE('',#7836,#7837,#1084,.T.);
#9649=EDGE_CURVE('',#7850,#7851,#7100,.T.);
#9650=EDGE_CURVE('',#7851,#7852,#1542,.T.);
#9651=EDGE_CURVE('',#7853,#7852,#7101,.T.);
#9652=EDGE_CURVE('',#7850,#7853,#1543,.T.);
#9653=EDGE_CURVE('',#7851,#7850,#7102,.T.);
#9654=EDGE_CURVE('',#7852,#7853,#7103,.T.);
#9655=EDGE_CURVE('',#7854,#7854,#7104,.T.);
#9656=EDGE_CURVE('',#7854,#7855,#1544,.T.);
#9657=EDGE_CURVE('',#7856,#7855,#1085,.T.);
#9658=EDGE_CURVE('',#7857,#7856,#1086,.T.);
#9659=EDGE_CURVE('',#7858,#7857,#1087,.T.);
#9660=EDGE_CURVE('',#7859,#7858,#1088,.T.);
#9661=EDGE_CURVE('',#7860,#7859,#1089,.T.);
#9662=EDGE_CURVE('',#7861,#7860,#1090,.T.);
#9663=EDGE_CURVE('',#7862,#7861,#1091,.T.);
#9664=EDGE_CURVE('',#7855,#7862,#1092,.T.);
#9665=EDGE_CURVE('',#7863,#7864,#7105,.T.);
#9666=EDGE_CURVE('',#7865,#7863,#1545,.T.);
#9667=EDGE_CURVE('',#7865,#7866,#7106,.T.);
#9668=EDGE_CURVE('',#7864,#7866,#1546,.T.);
#9669=EDGE_CURVE('',#7866,#7867,#7107,.T.);
#9670=EDGE_CURVE('',#7867,#7865,#7108,.T.);
#9671=EDGE_CURVE('',#7863,#7868,#7109,.T.);
#9672=EDGE_CURVE('',#7868,#7864,#7110,.T.);
#9673=EDGE_CURVE('',#7869,#7870,#7111,.T.);
#9674=EDGE_CURVE('',#7870,#7869,#7112,.T.);
#9675=EDGE_CURVE('',#7871,#7870,#1547,.T.);
#9676=EDGE_CURVE('',#7872,#7871,#7113,.T.);
#9677=EDGE_CURVE('',#7872,#7869,#1548,.T.);
#9678=EDGE_CURVE('',#7871,#7872,#7114,.T.);
#9679=EDGE_CURVE('',#7860,#7859,#1093,.T.);
#9680=EDGE_CURVE('',#7859,#7858,#1094,.T.);
#9681=EDGE_CURVE('',#7858,#7857,#1095,.T.);
#9682=EDGE_CURVE('',#7857,#7856,#1096,.T.);
#9683=EDGE_CURVE('',#7856,#7855,#1097,.T.);
#9684=EDGE_CURVE('',#7855,#7862,#1098,.T.);
#9685=EDGE_CURVE('',#7862,#7861,#1099,.T.);
#9686=EDGE_CURVE('',#7861,#7860,#1100,.T.);
#9687=EDGE_CURVE('',#7838,#7873,#1549,.T.);
#9688=EDGE_CURVE('',#7873,#7874,#1101,.T.);
#9689=EDGE_CURVE('',#7834,#7874,#1550,.T.);
#9690=EDGE_CURVE('',#7875,#7876,#7115,.T.);
#9691=EDGE_CURVE('',#7877,#7875,#1551,.T.);
#9692=EDGE_CURVE('',#7878,#7877,#7116,.T.);
#9693=EDGE_CURVE('',#7876,#7878,#1552,.T.);
#9694=EDGE_CURVE('',#7879,#7880,#7117,.T.);
#9695=EDGE_CURVE('',#7881,#7879,#1553,.T.);
#9696=EDGE_CURVE('',#7882,#7881,#7118,.T.);
#9697=EDGE_CURVE('',#7880,#7882,#1554,.T.);
#9698=EDGE_CURVE('',#7855,#7883,#1555,.T.);
#9699=EDGE_CURVE('',#7884,#7883,#1102,.T.);
#9700=EDGE_CURVE('',#7859,#7884,#1556,.T.);
#9701=EDGE_CURVE('',#7885,#7886,#7119,.T.);
#9702=EDGE_CURVE('',#7885,#7887,#1557,.T.);
#9703=EDGE_CURVE('',#7887,#7888,#7120,.T.);
#9704=EDGE_CURVE('',#7886,#7888,#1558,.T.);
#9705=EDGE_CURVE('',#7889,#7890,#7121,.T.);
#9706=EDGE_CURVE('',#7890,#7891,#1559,.T.);
#9707=EDGE_CURVE('',#7891,#7892,#7122,.T.);
#9708=EDGE_CURVE('',#7892,#7889,#1560,.T.);
#9709=EDGE_CURVE('',#7893,#7894,#7123,.T.);
#9710=EDGE_CURVE('',#7894,#7895,#1561,.T.);
#9711=EDGE_CURVE('',#7896,#7895,#7124,.T.);
#9712=EDGE_CURVE('',#7893,#7896,#1562,.T.);
#9713=EDGE_CURVE('',#7897,#7897,#7125,.T.);
#9714=EDGE_CURVE('',#7897,#7868,#1563,.T.);
#9715=EDGE_CURVE('',#7867,#7898,#1564,.T.);
#9716=EDGE_CURVE('',#7898,#7898,#7126,.T.);
#9717=EDGE_CURVE('',#7899,#7899,#7127,.T.);
#9718=EDGE_CURVE('',#7899,#7884,#1565,.T.);
#9719=EDGE_CURVE('',#7883,#7900,#1103,.F.);
#9720=EDGE_CURVE('',#7900,#7901,#1566,.T.);
#9721=EDGE_CURVE('',#7901,#7901,#7128,.T.);
#9722=EDGE_CURVE('',#7900,#7884,#1104,.F.);
#9723=EDGE_CURVE('',#7874,#7873,#1105,.T.);
#9724=EDGE_CURVE('',#7902,#7876,#7129,.T.);
#9725=EDGE_CURVE('',#7903,#7878,#7130,.T.);
#9726=EDGE_CURVE('',#7902,#7903,#1567,.T.);
#9727=EDGE_CURVE('',#7904,#7905,#1568,.T.);
#9728=EDGE_CURVE('',#7905,#7886,#7131,.T.);
#9729=EDGE_CURVE('',#7904,#7888,#7132,.T.);
#9730=EDGE_CURVE('',#7885,#7906,#7133,.T.);
#9731=EDGE_CURVE('',#7906,#7907,#1569,.T.);
#9732=EDGE_CURVE('',#7887,#7907,#7134,.T.);
#9733=EDGE_CURVE('',#7879,#7908,#7135,.T.);
#9734=EDGE_CURVE('',#7908,#7909,#1570,.T.);
#9735=EDGE_CURVE('',#7881,#7909,#7136,.T.);
#9736=EDGE_CURVE('',#7907,#7910,#7137,.T.);
#9737=EDGE_CURVE('',#7910,#7911,#7138,.T.);
#9738=EDGE_CURVE('',#7911,#7912,#7139,.T.);
#9739=EDGE_CURVE('',#7882,#7912,#7140,.T.);
#9740=EDGE_CURVE('',#7903,#7909,#7141,.T.);
#9741=EDGE_CURVE('',#7877,#7913,#7142,.T.);
#9742=EDGE_CURVE('',#7913,#7914,#7143,.T.);
#9743=EDGE_CURVE('',#7915,#7914,#7144,.T.);
#9744=EDGE_CURVE('',#7915,#7904,#7145,.T.);
#9745=EDGE_CURVE('',#7916,#7917,#1571,.T.);
#9746=EDGE_CURVE('',#7918,#7916,#1572,.T.);
#9747=EDGE_CURVE('',#7919,#7918,#7146,.T.);
#9748=EDGE_CURVE('',#7919,#7920,#1573,.T.);
#9749=EDGE_CURVE('',#7921,#7920,#1574,.T.);
#9750=EDGE_CURVE('',#7894,#7921,#1575,.T.);
#9751=EDGE_CURVE('',#7893,#7922,#1576,.T.);
#9752=EDGE_CURVE('',#7923,#7922,#1577,.T.);
#9753=EDGE_CURVE('',#7924,#7923,#1578,.T.);
#9754=EDGE_CURVE('',#7925,#7924,#7147,.T.);
#9755=EDGE_CURVE('',#7925,#7926,#1579,.T.);
#9756=EDGE_CURVE('',#7927,#7926,#1580,.T.);
#9757=EDGE_CURVE('',#7928,#7927,#1581,.T.);
#9758=EDGE_CURVE('',#7929,#7928,#7148,.T.);
#9759=EDGE_CURVE('',#7929,#7930,#1582,.T.);
#9760=EDGE_CURVE('',#7931,#7930,#1583,.T.);
#9761=EDGE_CURVE('',#7932,#7931,#1584,.T.);
#9762=EDGE_CURVE('',#7933,#7932,#7149,.T.);
#9763=EDGE_CURVE('',#7933,#7934,#1585,.T.);
#9764=EDGE_CURVE('',#7935,#7934,#1586,.T.);
#9765=EDGE_CURVE('',#7936,#7935,#1587,.T.);
#9766=EDGE_CURVE('',#7936,#7937,#1588,.T.);
#9767=EDGE_CURVE('',#7938,#7937,#7150,.T.);
#9768=EDGE_CURVE('',#7938,#7939,#1589,.T.);
#9769=EDGE_CURVE('',#7939,#7940,#1590,.T.);
#9770=EDGE_CURVE('',#7941,#7940,#1591,.T.);
#9771=EDGE_CURVE('',#7942,#7941,#1592,.T.);
#9772=EDGE_CURVE('',#7942,#7943,#1593,.T.);
#9773=EDGE_CURVE('',#7944,#7943,#7151,.T.);
#9774=EDGE_CURVE('',#7944,#7945,#1594,.T.);
#9775=EDGE_CURVE('',#7946,#7945,#1595,.T.);
#9776=EDGE_CURVE('',#7947,#7946,#1596,.T.);
#9777=EDGE_CURVE('',#7948,#7947,#7152,.T.);
#9778=EDGE_CURVE('',#7948,#7949,#1597,.T.);
#9779=EDGE_CURVE('',#7950,#7949,#1598,.T.);
#9780=EDGE_CURVE('',#7951,#7950,#1599,.T.);
#9781=EDGE_CURVE('',#7952,#7951,#7153,.T.);
#9782=EDGE_CURVE('',#7952,#7917,#1600,.T.);
#9783=EDGE_CURVE('',#7918,#7953,#1601,.T.);
#9784=EDGE_CURVE('',#7954,#7953,#7154,.T.);
#9785=EDGE_CURVE('',#7919,#7954,#1602,.T.);
#9786=EDGE_CURVE('',#7924,#7955,#1603,.T.);
#9787=EDGE_CURVE('',#7956,#7955,#7155,.T.);
#9788=EDGE_CURVE('',#7925,#7956,#1604,.T.);
#9789=EDGE_CURVE('',#7928,#7957,#1605,.T.);
#9790=EDGE_CURVE('',#7958,#7957,#7156,.T.);
#9791=EDGE_CURVE('',#7929,#7958,#1606,.T.);
#9792=EDGE_CURVE('',#7932,#7959,#1607,.T.);
#9793=EDGE_CURVE('',#7960,#7959,#7157,.T.);
#9794=EDGE_CURVE('',#7933,#7960,#1608,.T.);
#9795=EDGE_CURVE('',#7937,#7961,#1609,.T.);
#9796=EDGE_CURVE('',#7962,#7961,#7158,.T.);
#9797=EDGE_CURVE('',#7962,#7938,#1610,.T.);
#9798=EDGE_CURVE('',#7952,#7963,#1611,.T.);
#9799=EDGE_CURVE('',#7951,#7964,#1612,.T.);
#9800=EDGE_CURVE('',#7963,#7964,#7159,.T.);
#9801=EDGE_CURVE('',#7943,#7965,#1613,.T.);
#9802=EDGE_CURVE('',#7966,#7965,#7160,.T.);
#9803=EDGE_CURVE('',#7944,#7966,#1614,.T.);
#9804=EDGE_CURVE('',#7947,#7967,#1615,.T.);
#9805=EDGE_CURVE('',#7968,#7967,#7161,.T.);
#9806=EDGE_CURVE('',#7948,#7968,#1616,.T.);
#9807=EDGE_CURVE('',#7910,#7969,#1617,.T.);
#9808=EDGE_CURVE('',#7969,#7970,#7162,.T.);
#9809=EDGE_CURVE('',#7911,#7970,#1618,.T.);
#9810=EDGE_CURVE('',#7970,#7971,#7163,.T.);
#9811=EDGE_CURVE('',#7912,#7971,#1619,.T.);
#9812=EDGE_CURVE('',#7880,#7971,#7164,.T.);
#9813=EDGE_CURVE('',#7875,#7972,#7165,.T.);
#9814=EDGE_CURVE('',#7913,#7972,#1620,.T.);
#9815=EDGE_CURVE('',#7972,#7973,#7166,.T.);
#9816=EDGE_CURVE('',#7914,#7973,#1621,.T.);
#9817=EDGE_CURVE('',#7974,#7973,#7167,.T.);
#9818=EDGE_CURVE('',#7974,#7915,#1622,.T.);
#9819=EDGE_CURVE('',#7905,#7974,#7168,.T.);
#9820=EDGE_CURVE('',#7902,#7908,#7169,.T.);
#9821=EDGE_CURVE('',#7969,#7906,#7170,.T.);
#9822=EDGE_CURVE('',#7889,#7975,#1623,.T.);
#9823=EDGE_CURVE('',#7975,#7976,#1624,.T.);
#9824=EDGE_CURVE('',#7976,#7890,#1625,.T.);
#9825=EDGE_CURVE('',#7977,#7953,#1626,.T.);
#9826=EDGE_CURVE('',#7977,#7978,#1627,.T.);
#9827=EDGE_CURVE('',#7978,#7963,#1628,.T.);
#9828=EDGE_CURVE('',#7979,#7964,#1629,.T.);
#9829=EDGE_CURVE('',#7979,#7980,#1630,.T.);
#9830=EDGE_CURVE('',#7980,#7968,#1631,.T.);
#9831=EDGE_CURVE('',#7981,#7967,#1632,.T.);
#9832=EDGE_CURVE('',#7981,#7982,#1633,.T.);
#9833=EDGE_CURVE('',#7982,#7966,#1634,.T.);
#9834=EDGE_CURVE('',#7983,#7965,#1635,.T.);
#9835=EDGE_CURVE('',#7984,#7983,#1636,.T.);
#9836=EDGE_CURVE('',#7984,#7985,#1637,.T.);
#9837=EDGE_CURVE('',#7985,#7986,#1638,.T.);
#9838=EDGE_CURVE('',#7962,#7986,#1639,.T.);
#9839=EDGE_CURVE('',#7987,#7961,#1640,.T.);
#9840=EDGE_CURVE('',#7988,#7987,#1641,.T.);
#9841=EDGE_CURVE('',#7988,#7989,#1642,.T.);
#9842=EDGE_CURVE('',#7989,#7960,#1643,.T.);
#9843=EDGE_CURVE('',#7990,#7959,#1644,.T.);
#9844=EDGE_CURVE('',#7990,#7991,#1645,.T.);
#9845=EDGE_CURVE('',#7991,#7958,#1646,.T.);
#9846=EDGE_CURVE('',#7992,#7957,#1647,.T.);
#9847=EDGE_CURVE('',#7992,#7993,#1648,.T.);
#9848=EDGE_CURVE('',#7993,#7956,#1649,.T.);
#9849=EDGE_CURVE('',#7994,#7955,#1650,.T.);
#9850=EDGE_CURVE('',#7994,#7995,#1651,.T.);
#9851=EDGE_CURVE('',#7995,#7896,#1652,.T.);
#9852=EDGE_CURVE('',#7996,#7895,#1653,.T.);
#9853=EDGE_CURVE('',#7996,#7997,#1654,.T.);
#9854=EDGE_CURVE('',#7997,#7954,#1655,.T.);
#9855=EDGE_CURVE('',#7892,#7998,#1656,.T.);
#9856=EDGE_CURVE('',#7999,#7891,#1657,.T.);
#9857=EDGE_CURVE('',#7998,#7999,#1658,.T.);
#9858=EDGE_CURVE('',#7949,#7980,#1659,.T.);
#9859=EDGE_CURVE('',#7950,#7979,#1660,.T.);
#9860=EDGE_CURVE('',#7945,#7982,#1661,.T.);
#9861=EDGE_CURVE('',#7946,#7981,#1662,.T.);
#9862=EDGE_CURVE('',#7986,#7939,#1663,.T.);
#9863=EDGE_CURVE('',#7983,#7942,#1664,.T.);
#9864=EDGE_CURVE('',#7940,#7985,#1665,.T.);
#9865=EDGE_CURVE('',#7941,#7984,#1666,.T.);
#9866=EDGE_CURVE('',#7987,#7936,#1667,.T.);
#9867=EDGE_CURVE('',#7934,#7989,#1668,.T.);
#9868=EDGE_CURVE('',#7935,#7988,#1669,.T.);
#9869=EDGE_CURVE('',#7930,#7991,#1670,.T.);
#9870=EDGE_CURVE('',#7931,#7990,#1671,.T.);
#9871=EDGE_CURVE('',#7926,#7993,#1672,.T.);
#9872=EDGE_CURVE('',#7927,#7992,#1673,.T.);
#9873=EDGE_CURVE('',#7922,#7995,#1674,.T.);
#9874=EDGE_CURVE('',#7923,#7994,#1675,.T.);
#9875=EDGE_CURVE('',#7920,#7997,#1676,.T.);
#9876=EDGE_CURVE('',#7921,#7996,#1677,.T.);
#9877=EDGE_CURVE('',#7917,#7978,#1678,.T.);
#9878=EDGE_CURVE('',#7916,#7977,#1679,.T.);
#9879=EDGE_CURVE('',#7975,#7998,#1680,.T.);
#9880=EDGE_CURVE('',#7976,#7999,#1681,.T.);
#9881=EDGE_CURVE('',#8000,#8001,#7171,.T.);
#9882=EDGE_CURVE('',#8000,#8002,#7172,.T.);
#9883=EDGE_CURVE('',#8003,#8002,#1106,.T.);
#9884=EDGE_CURVE('',#8004,#8003,#1107,.T.);
#9885=EDGE_CURVE('',#8004,#8005,#7173,.T.);
#9886=EDGE_CURVE('',#8005,#8006,#7174,.T.);
#9887=EDGE_CURVE('',#8006,#8005,#7175,.T.);
#9888=EDGE_CURVE('',#8007,#8004,#1108,.T.);
#9889=EDGE_CURVE('',#8002,#8007,#1109,.T.);
#9890=EDGE_CURVE('',#8001,#8000,#7176,.T.);
#9891=EDGE_CURVE('',#8008,#8009,#7177,.T.);
#9892=EDGE_CURVE('',#8009,#8008,#7178,.T.);
#9893=EDGE_CURVE('',#8009,#8010,#7179,.T.);
#9894=EDGE_CURVE('',#8010,#8011,#1110,.T.);
#9895=EDGE_CURVE('',#8011,#8012,#1111,.T.);
#9896=EDGE_CURVE('',#8012,#8013,#7180,.T.);
#9897=EDGE_CURVE('',#8013,#8014,#7181,.T.);
#9898=EDGE_CURVE('',#8014,#8013,#7182,.T.);
#9899=EDGE_CURVE('',#8012,#8015,#1112,.T.);
#9900=EDGE_CURVE('',#8015,#8010,#1113,.T.);
#9901=EDGE_CURVE('',#8016,#8017,#1114,.T.);
#9902=EDGE_CURVE('',#8017,#8003,#7183,.T.);
#9903=EDGE_CURVE('',#8016,#8007,#7184,.T.);
#9904=EDGE_CURVE('',#8006,#8018,#1682,.T.);
#9905=EDGE_CURVE('',#8018,#8018,#7185,.T.);
#9906=EDGE_CURVE('',#8019,#8019,#7186,.T.);
#9907=EDGE_CURVE('',#8019,#8001,#1683,.T.);
#9908=EDGE_CURVE('',#8020,#8021,#1115,.T.);
#9909=EDGE_CURVE('',#8020,#8011,#7187,.T.);
#9910=EDGE_CURVE('',#8021,#8015,#7188,.T.);
#9911=EDGE_CURVE('',#8022,#8022,#7189,.T.);
#9912=EDGE_CURVE('',#8022,#8008,#1684,.T.);
#9913=EDGE_CURVE('',#8014,#8023,#1685,.T.);
#9914=EDGE_CURVE('',#8023,#8023,#7190,.T.);
#9915=EDGE_CURVE('',#8021,#8020,#1116,.T.);
#9916=EDGE_CURVE('',#8017,#8016,#1117,.T.);
#9917=EDGE_CURVE('',#8024,#8024,#7191,.T.);
#9918=EDGE_CURVE('',#8024,#8025,#1686,.T.);
#9919=EDGE_CURVE('',#8025,#8025,#7192,.T.);
#9920=EDGE_CURVE('',#8026,#8026,#7193,.T.);
#9921=EDGE_CURVE('',#8026,#8027,#1687,.T.);
#9922=EDGE_CURVE('',#8027,#8027,#7194,.T.);
#9923=EDGE_CURVE('',#8028,#8028,#7195,.T.);
#9924=EDGE_CURVE('',#8028,#8029,#1688,.T.);
#9925=EDGE_CURVE('',#8029,#8029,#7196,.T.);
#9926=EDGE_CURVE('',#8030,#8030,#7197,.T.);
#9927=EDGE_CURVE('',#8030,#8031,#1689,.T.);
#9928=EDGE_CURVE('',#8031,#8031,#7198,.T.);
#9929=EDGE_CURVE('',#8032,#8033,#1690,.T.);
#9930=EDGE_CURVE('',#8034,#8032,#1691,.T.);
#9931=EDGE_CURVE('',#8035,#8034,#1692,.T.);
#9932=EDGE_CURVE('',#8036,#8035,#1693,.T.);
#9933=EDGE_CURVE('',#8037,#8036,#1694,.T.);
#9934=EDGE_CURVE('',#8038,#8037,#1695,.T.);
#9935=EDGE_CURVE('',#8039,#8038,#1696,.T.);
#9936=EDGE_CURVE('',#8039,#8040,#1697,.T.);
#9937=EDGE_CURVE('',#8040,#8041,#1698,.T.);
#9938=EDGE_CURVE('',#8042,#8041,#1699,.T.);
#9939=EDGE_CURVE('',#8043,#8042,#1700,.T.);
#9940=EDGE_CURVE('',#8033,#8043,#1701,.T.);
#9941=EDGE_CURVE('',#8044,#8045,#1702,.T.);
#9942=EDGE_CURVE('',#8046,#8044,#1703,.T.);
#9943=EDGE_CURVE('',#8046,#8047,#1704,.T.);
#9944=EDGE_CURVE('',#8047,#8048,#1705,.T.);
#9945=EDGE_CURVE('',#8048,#8049,#1706,.T.);
#9946=EDGE_CURVE('',#8049,#8050,#1707,.T.);
#9947=EDGE_CURVE('',#8051,#8050,#1708,.T.);
#9948=EDGE_CURVE('',#8051,#8052,#1709,.T.);
#9949=EDGE_CURVE('',#8052,#8053,#1710,.T.);
#9950=EDGE_CURVE('',#8053,#8054,#1711,.T.);
#9951=EDGE_CURVE('',#8054,#8055,#1712,.T.);
#9952=EDGE_CURVE('',#8045,#8055,#1713,.T.);
#9953=EDGE_CURVE('',#8056,#8038,#1714,.T.);
#9954=EDGE_CURVE('',#8057,#8056,#1715,.T.);
#9955=EDGE_CURVE('',#8057,#8039,#1716,.T.);
#9956=EDGE_CURVE('',#8058,#8056,#1717,.T.);
#9957=EDGE_CURVE('',#8059,#8058,#1718,.T.);
#9958=EDGE_CURVE('',#8059,#8057,#1719,.T.);
#9959=EDGE_CURVE('',#8060,#8058,#1720,.T.);
#9960=EDGE_CURVE('',#8061,#8060,#1721,.T.);
#9961=EDGE_CURVE('',#8061,#8059,#1722,.T.);
#9962=EDGE_CURVE('',#8062,#8060,#1723,.T.);
#9963=EDGE_CURVE('',#8063,#8062,#1724,.T.);
#9964=EDGE_CURVE('',#8063,#8061,#1725,.T.);
#9965=EDGE_CURVE('',#8053,#8062,#1726,.T.);
#9966=EDGE_CURVE('',#8052,#8063,#1727,.T.);
#9967=EDGE_CURVE('',#8064,#8050,#1728,.T.);
#9968=EDGE_CURVE('',#8065,#8064,#1729,.T.);
#9969=EDGE_CURVE('',#8065,#8051,#1730,.T.);
#9970=EDGE_CURVE('',#8066,#8064,#1731,.T.);
#9971=EDGE_CURVE('',#8067,#8066,#1732,.T.);
#9972=EDGE_CURVE('',#8067,#8065,#1733,.T.);
#9973=EDGE_CURVE('',#8068,#8066,#1734,.T.);
#9974=EDGE_CURVE('',#8069,#8068,#1735,.T.);
#9975=EDGE_CURVE('',#8069,#8067,#1736,.T.);
#9976=EDGE_CURVE('',#8070,#8068,#1737,.T.);
#9977=EDGE_CURVE('',#8071,#8070,#1738,.T.);
#9978=EDGE_CURVE('',#8071,#8069,#1739,.T.);
#9979=EDGE_CURVE('',#8041,#8070,#1740,.T.);
#9980=EDGE_CURVE('',#8040,#8071,#1741,.T.);
#9981=EDGE_CURVE('',#8072,#8037,#1742,.T.);
#9982=EDGE_CURVE('',#8073,#8072,#1743,.T.);
#9983=EDGE_CURVE('',#8073,#8041,#1744,.T.);
#9984=EDGE_CURVE('',#8074,#8050,#1745,.T.);
#9985=EDGE_CURVE('',#8074,#8075,#1746,.T.);
#9986=EDGE_CURVE('',#8075,#8054,#1747,.T.);
#9987=EDGE_CURVE('',#8076,#8073,#1748,.T.);
#9988=EDGE_CURVE('',#8076,#8042,#1749,.T.);
#9989=EDGE_CURVE('',#8077,#8036,#1750,.T.);
#9990=EDGE_CURVE('',#8072,#8077,#1751,.T.);
#9991=EDGE_CURVE('',#8045,#8035,#1752,.T.);
#9992=EDGE_CURVE('',#8078,#8055,#1753,.T.);
#9993=EDGE_CURVE('',#8078,#8079,#1754,.T.);
#9994=EDGE_CURVE('',#8080,#8079,#1755,.T.);
#9995=EDGE_CURVE('',#8077,#8080,#1756,.T.);
#9996=EDGE_CURVE('',#8079,#8081,#1757,.T.);
#9997=EDGE_CURVE('',#8081,#8047,#1758,.T.);
#9998=EDGE_CURVE('',#8046,#8032,#1759,.T.);
#9999=EDGE_CURVE('',#8082,#8033,#1760,.T.);
#10000=EDGE_CURVE('',#8080,#8082,#1761,.T.);
#10001=EDGE_CURVE('',#8083,#8043,#1762,.T.);
#10002=EDGE_CURVE('',#8082,#8083,#1763,.T.);
#10003=EDGE_CURVE('',#8083,#8076,#1764,.T.);
#10004=EDGE_CURVE('',#8084,#8049,#1765,.T.);
#10005=EDGE_CURVE('',#8084,#8074,#1766,.T.);
#10006=EDGE_CURVE('',#8085,#8048,#1767,.T.);
#10007=EDGE_CURVE('',#8085,#8084,#1768,.T.);
#10008=EDGE_CURVE('',#8081,#8085,#1769,.T.);
#10009=EDGE_CURVE('',#8075,#8078,#1770,.T.);
#10010=EDGE_CURVE('',#8044,#8034,#1771,.T.);
#10011=EDGE_CURVE('',#8086,#8086,#7199,.T.);
#10012=EDGE_CURVE('',#8086,#8087,#1772,.T.);
#10013=EDGE_CURVE('',#8087,#8087,#7200,.T.);
#10014=EDGE_CURVE('',#8088,#8088,#7201,.T.);
#10015=EDGE_CURVE('',#8088,#8089,#1773,.T.);
#10016=EDGE_CURVE('',#8089,#8089,#7202,.T.);
#10017=EDGE_CURVE('',#8090,#8090,#7203,.T.);
#10018=EDGE_CURVE('',#8090,#8091,#1774,.T.);
#10019=EDGE_CURVE('',#8091,#8091,#7204,.T.);
#10020=EDGE_CURVE('',#8092,#8092,#7205,.T.);
#10021=EDGE_CURVE('',#8092,#8093,#1775,.T.);
#10022=EDGE_CURVE('',#8093,#8093,#7206,.T.);
#10023=EDGE_CURVE('',#8094,#8094,#7207,.T.);
#10024=EDGE_CURVE('',#8094,#8095,#1776,.T.);
#10025=EDGE_CURVE('',#8095,#8095,#7208,.T.);
#10026=EDGE_CURVE('',#8096,#8096,#7209,.T.);
#10027=EDGE_CURVE('',#8096,#8097,#1777,.T.);
#10028=EDGE_CURVE('',#8097,#8097,#7210,.T.);
#10029=EDGE_CURVE('',#8098,#8098,#7211,.T.);
#10030=EDGE_CURVE('',#8098,#8099,#1778,.T.);
#10031=EDGE_CURVE('',#8099,#8099,#7212,.T.);
#10032=EDGE_CURVE('',#8100,#8100,#7213,.T.);
#10033=EDGE_CURVE('',#8100,#8101,#1779,.T.);
#10034=EDGE_CURVE('',#8101,#8101,#7214,.T.);
#10035=EDGE_CURVE('',#8102,#8102,#7215,.T.);
#10036=EDGE_CURVE('',#8102,#8103,#1780,.T.);
#10037=EDGE_CURVE('',#8103,#8103,#7216,.T.);
#10038=EDGE_CURVE('',#8104,#8104,#7217,.T.);
#10039=EDGE_CURVE('',#8104,#8105,#1781,.T.);
#10040=EDGE_CURVE('',#8105,#8105,#7218,.T.);
#10041=EDGE_CURVE('',#8106,#8106,#7219,.T.);
#10042=EDGE_CURVE('',#8106,#8107,#1782,.T.);
#10043=EDGE_CURVE('',#8107,#8107,#7220,.T.);
#10044=EDGE_CURVE('',#8108,#8108,#7221,.T.);
#10045=EDGE_CURVE('',#8108,#8109,#1783,.T.);
#10046=EDGE_CURVE('',#8109,#8109,#7222,.T.);
#10047=EDGE_CURVE('',#8110,#8110,#7223,.T.);
#10048=EDGE_CURVE('',#8110,#8111,#1784,.T.);
#10049=EDGE_CURVE('',#8111,#8111,#7224,.T.);
#10050=EDGE_CURVE('',#8112,#8112,#7225,.T.);
#10051=EDGE_CURVE('',#8112,#8113,#1785,.T.);
#10052=EDGE_CURVE('',#8113,#8113,#7226,.T.);
#10053=EDGE_CURVE('',#8114,#8114,#7227,.T.);
#10054=EDGE_CURVE('',#8114,#8115,#1786,.T.);
#10055=EDGE_CURVE('',#8115,#8115,#7228,.T.);
#10056=EDGE_CURVE('',#8116,#8116,#7229,.T.);
#10057=EDGE_CURVE('',#8116,#8117,#1787,.T.);
#10058=EDGE_CURVE('',#8117,#8117,#7230,.T.);
#10059=EDGE_CURVE('',#8118,#8118,#7231,.T.);
#10060=EDGE_CURVE('',#8118,#8119,#1788,.T.);
#10061=EDGE_CURVE('',#8119,#8119,#7232,.T.);
#10062=EDGE_CURVE('',#8120,#8120,#7233,.T.);
#10063=EDGE_CURVE('',#8120,#8121,#1789,.T.);
#10064=EDGE_CURVE('',#8121,#8121,#7234,.T.);
#10065=EDGE_CURVE('',#8122,#8122,#7235,.T.);
#10066=EDGE_CURVE('',#8122,#8123,#7236,.T.);
#10067=EDGE_CURVE('',#8124,#8123,#7237,.T.);
#10068=EDGE_CURVE('',#8123,#8124,#7238,.T.);
#10069=EDGE_CURVE('',#8125,#8126,#7239,.T.);
#10070=EDGE_CURVE('',#8125,#8127,#7240,.T.);
#10071=EDGE_CURVE('',#8127,#8128,#7241,.T.);
#10072=EDGE_CURVE('',#8128,#8127,#7242,.T.);
#10073=EDGE_CURVE('',#8126,#8125,#7243,.T.);
#10074=EDGE_CURVE('',#8129,#8130,#7244,.T.);
#10075=EDGE_CURVE('',#8129,#8131,#7245,.T.);
#10076=EDGE_CURVE('',#8131,#8132,#7246,.T.);
#10077=EDGE_CURVE('',#8132,#8131,#7247,.T.);
#10078=EDGE_CURVE('',#8130,#8129,#7248,.T.);
#10079=EDGE_CURVE('',#8133,#8134,#7249,.T.);
#10080=EDGE_CURVE('',#8133,#8135,#7250,.T.);
#10081=EDGE_CURVE('',#8136,#8135,#7251,.T.);
#10082=EDGE_CURVE('',#8135,#8136,#7252,.T.);
#10083=EDGE_CURVE('',#8134,#8133,#7253,.T.);
#10084=EDGE_CURVE('',#8137,#8137,#7254,.T.);
#10085=EDGE_CURVE('',#8137,#8138,#1790,.T.);
#10086=EDGE_CURVE('',#8138,#8138,#7255,.T.);
#10087=EDGE_CURVE('',#8126,#8124,#1791,.T.);
#10088=EDGE_CURVE('',#8132,#8139,#1792,.T.);
#10089=EDGE_CURVE('',#8139,#8139,#7256,.T.);
#10090=EDGE_CURVE('',#8134,#8128,#1793,.T.);
#10091=EDGE_CURVE('',#8130,#8136,#1794,.T.);
#10092=EDGE_CURVE('',#8140,#8141,#7257,.T.);
#10093=EDGE_CURVE('',#8141,#8140,#7258,.T.);
#10094=EDGE_CURVE('',#8140,#8142,#1795,.T.);
#10095=EDGE_CURVE('',#8142,#8142,#7259,.T.);
#10096=EDGE_CURVE('',#8141,#8143,#1796,.T.);
#10097=EDGE_CURVE('',#8143,#8143,#7260,.T.);
#10098=EDGE_CURVE('',#8144,#8145,#1797,.T.);
#10099=EDGE_CURVE('',#8145,#8145,#7261,.T.);
#10100=EDGE_CURVE('',#8146,#8147,#1798,.T.);
#10101=EDGE_CURVE('',#8147,#8148,#1799,.T.);
#10102=EDGE_CURVE('',#8148,#8149,#1800,.T.);
#10103=EDGE_CURVE('',#8149,#8150,#1801,.T.);
#10104=EDGE_CURVE('',#8150,#8151,#1802,.T.);
#10105=EDGE_CURVE('',#8151,#8146,#1803,.T.);
#10106=EDGE_CURVE('',#8148,#8152,#1804,.T.);
#10107=EDGE_CURVE('',#8153,#8147,#1805,.T.);
#10108=EDGE_CURVE('',#8152,#8153,#1806,.T.);
#10109=EDGE_CURVE('',#8154,#8146,#1807,.T.);
#10110=EDGE_CURVE('',#8153,#8154,#1808,.T.);
#10111=EDGE_CURVE('',#8155,#8151,#1809,.T.);
#10112=EDGE_CURVE('',#8156,#8155,#1810,.T.);
#10113=EDGE_CURVE('',#8154,#8156,#1811,.T.);
#10114=EDGE_CURVE('',#8157,#8150,#1812,.T.);
#10115=EDGE_CURVE('',#8155,#8157,#1813,.T.);
#10116=EDGE_CURVE('',#8158,#8149,#1814,.T.);
#10117=EDGE_CURVE('',#8157,#8158,#1815,.T.);
#10118=EDGE_CURVE('',#8158,#8159,#1816,.T.);
#10119=EDGE_CURVE('',#8159,#8152,#1817,.T.);
#10120=EDGE_CURVE('',#8156,#8159,#1818,.T.);
#10121=EDGE_CURVE('',#8160,#8161,#97,.T.);
#10122=EDGE_CURVE('',#8160,#8162,#1819,.T.);
#10123=EDGE_CURVE('',#8162,#8163,#1118,.T.);
#10124=EDGE_CURVE('',#8163,#8164,#1119,.T.);
#10125=EDGE_CURVE('',#8161,#8164,#1820,.T.);
#10126=EDGE_CURVE('',#8165,#8160,#98,.T.);
#10127=EDGE_CURVE('',#8165,#8166,#1821,.T.);
#10128=EDGE_CURVE('',#8166,#8167,#1120,.T.);
#10129=EDGE_CURVE('',#8167,#8168,#1121,.T.);
#10130=EDGE_CURVE('',#8168,#8162,#1122,.T.);
#10131=EDGE_CURVE('',#8169,#8169,#7262,.T.);
#10132=EDGE_CURVE('',#8169,#8170,#7263,.T.);
#10133=EDGE_CURVE('',#8170,#8171,#7264,.T.);
#10134=EDGE_CURVE('',#8171,#8170,#7265,.T.);
#10135=EDGE_CURVE('',#8172,#8172,#7266,.T.);
#10136=EDGE_CURVE('',#8172,#8173,#1822,.T.);
#10137=EDGE_CURVE('',#8173,#8173,#7267,.T.);
#10138=EDGE_CURVE('',#8174,#8174,#7268,.T.);
#10139=EDGE_CURVE('',#8174,#8175,#1823,.T.);
#10140=EDGE_CURVE('',#8175,#8175,#7269,.T.);
#10141=EDGE_CURVE('',#8176,#8176,#7270,.T.);
#10142=EDGE_CURVE('',#8176,#8177,#1824,.T.);
#10143=EDGE_CURVE('',#8177,#8177,#7271,.T.);
#10144=EDGE_CURVE('',#8178,#8178,#7272,.T.);
#10145=EDGE_CURVE('',#8178,#8179,#1825,.T.);
#10146=EDGE_CURVE('',#8179,#8179,#7273,.T.);
#10147=EDGE_CURVE('',#8180,#8181,#7274,.T.);
#10148=EDGE_CURVE('',#8182,#8180,#1377,.T.);
#10149=EDGE_CURVE('',#8182,#8183,#1826,.T.);
#10150=EDGE_CURVE('',#8183,#8183,#7275,.T.);
#10151=EDGE_CURVE('',#8181,#8182,#1378,.T.);
#10152=EDGE_CURVE('',#8184,#8185,#7276,.T.);
#10153=EDGE_CURVE('',#8185,#8186,#1123,.T.);
#10154=EDGE_CURVE('',#8186,#8187,#7277,.T.);
#10155=EDGE_CURVE('',#8187,#8184,#1124,.T.);
#10156=EDGE_CURVE('',#8188,#8189,#7278,.T.);
#10157=EDGE_CURVE('',#8189,#8190,#1125,.T.);
#10158=EDGE_CURVE('',#8191,#8190,#7279,.T.);
#10159=EDGE_CURVE('',#8191,#8192,#1126,.T.);
#10160=EDGE_CURVE('',#8192,#8186,#7280,.T.);
#10161=EDGE_CURVE('',#8185,#8193,#7281,.T.);
#10162=EDGE_CURVE('',#8193,#8188,#1127,.T.);
#10163=EDGE_CURVE('',#8191,#8194,#7282,.T.);
#10164=EDGE_CURVE('',#8194,#8195,#1128,.T.);
#10165=EDGE_CURVE('',#8195,#8192,#7283,.T.);
#10166=EDGE_CURVE('',#8196,#8196,#7284,.T.);
#10167=EDGE_CURVE('',#8196,#8197,#1827,.T.);
#10168=EDGE_CURVE('',#8197,#8197,#7285,.T.);
#10169=EDGE_CURVE('',#8198,#8198,#7286,.T.);
#10170=EDGE_CURVE('',#8198,#8199,#1828,.T.);
#10171=EDGE_CURVE('',#8199,#8200,#1129,.T.);
#10172=EDGE_CURVE('',#8201,#8200,#7287,.T.);
#10173=EDGE_CURVE('',#8201,#8202,#1130,.T.);
#10174=EDGE_CURVE('',#8203,#8202,#7288,.T.);
#10175=EDGE_CURVE('',#8203,#8204,#1131,.T.);
#10176=EDGE_CURVE('',#8205,#8204,#7289,.T.);
#10177=EDGE_CURVE('',#8205,#8199,#1132,.T.);
#10178=EDGE_CURVE('',#8206,#8207,#7290,.T.);
#10179=EDGE_CURVE('',#8208,#8206,#1379,.T.);
#10180=EDGE_CURVE('',#8208,#8209,#7291,.T.);
#10181=EDGE_CURVE('',#8209,#8210,#1829,.T.);
#10182=EDGE_CURVE('',#8210,#8210,#7292,.T.);
#10183=EDGE_CURVE('',#8209,#8211,#7293,.T.);
#10184=EDGE_CURVE('',#8207,#8211,#1380,.T.);
#10185=EDGE_CURVE('',#8212,#8212,#7294,.T.);
#10186=EDGE_CURVE('',#8212,#8213,#1830,.T.);
#10187=EDGE_CURVE('',#8213,#8213,#7295,.T.);
#10188=EDGE_CURVE('',#8214,#8214,#7296,.T.);
#10189=EDGE_CURVE('',#8214,#8215,#1831,.T.);
#10190=EDGE_CURVE('',#8215,#8215,#7297,.T.);
#10191=EDGE_CURVE('',#8216,#8217,#1133,.F.);
#10192=EDGE_CURVE('',#8218,#8216,#1832,.T.);
#10193=EDGE_CURVE('',#8219,#8218,#1134,.F.);
#10194=EDGE_CURVE('',#8217,#8219,#1833,.T.);
#10195=EDGE_CURVE('',#8220,#8221,#1135,.F.);
#10196=EDGE_CURVE('',#8222,#8220,#1834,.T.);
#10197=EDGE_CURVE('',#8223,#8222,#1136,.F.);
#10198=EDGE_CURVE('',#8221,#8223,#1835,.T.);
#10199=EDGE_CURVE('',#8224,#8225,#1381,.T.);
#10200=EDGE_CURVE('',#8226,#8224,#1137,.T.);
#10201=EDGE_CURVE('',#8227,#8226,#1836,.T.);
#10202=EDGE_CURVE('',#8228,#8227,#1138,.T.);
#10203=EDGE_CURVE('',#8229,#8228,#1382,.T.);
#10204=EDGE_CURVE('',#8230,#8229,#1139,.T.);
#10205=EDGE_CURVE('',#8231,#8230,#1837,.T.);
#10206=EDGE_CURVE('',#8225,#8231,#1140,.T.);
#10207=EDGE_CURVE('',#8232,#8233,#1141,.F.);
#10208=EDGE_CURVE('',#8234,#8232,#1838,.T.);
#10209=EDGE_CURVE('',#8235,#8234,#7298,.T.);
#10210=EDGE_CURVE('',#8233,#8235,#1839,.T.);
#10211=EDGE_CURVE('',#8236,#8237,#1142,.F.);
#10212=EDGE_CURVE('',#8238,#8236,#1840,.T.);
#10213=EDGE_CURVE('',#8239,#8238,#1143,.F.);
#10214=EDGE_CURVE('',#8237,#8239,#1841,.T.);
#10215=EDGE_CURVE('',#8240,#8241,#7299,.T.);
#10216=EDGE_CURVE('',#8241,#8242,#7300,.T.);
#10217=EDGE_CURVE('',#8242,#8243,#1842,.T.);
#10218=EDGE_CURVE('',#8243,#8244,#7301,.T.);
#10219=EDGE_CURVE('',#8240,#8244,#1843,.T.);
#10220=EDGE_CURVE('',#8245,#8245,#7302,.T.);
#10221=EDGE_CURVE('',#8245,#8246,#1844,.T.);
#10222=EDGE_CURVE('',#8246,#8246,#7303,.T.);
#10223=EDGE_CURVE('',#8247,#8247,#7304,.T.);
#10224=EDGE_CURVE('',#8247,#8248,#1845,.T.);
#10225=EDGE_CURVE('',#8248,#8248,#7305,.T.);
#10226=EDGE_CURVE('',#8249,#8249,#7306,.T.);
#10227=EDGE_CURVE('',#8249,#8250,#1846,.T.);
#10228=EDGE_CURVE('',#8250,#8250,#7307,.T.);
#10229=EDGE_CURVE('',#8251,#8251,#7308,.T.);
#10230=EDGE_CURVE('',#8251,#8252,#1847,.T.);
#10231=EDGE_CURVE('',#8252,#8252,#7309,.T.);
#10232=EDGE_CURVE('',#8253,#8253,#7310,.T.);
#10233=EDGE_CURVE('',#8253,#8254,#1848,.T.);
#10234=EDGE_CURVE('',#8254,#8254,#7311,.T.);
#10235=EDGE_CURVE('',#8255,#8256,#7312,.T.);
#10236=EDGE_CURVE('',#8257,#8255,#1849,.T.);
#10237=EDGE_CURVE('',#8258,#8257,#1144,.F.);
#10238=EDGE_CURVE('',#8256,#8258,#1850,.T.);
#10239=EDGE_CURVE('',#8259,#8260,#7313,.T.);
#10240=EDGE_CURVE('',#8261,#8259,#1851,.T.);
#10241=EDGE_CURVE('',#8262,#8261,#1145,.F.);
#10242=EDGE_CURVE('',#8226,#8262,#1146,.F.);
#10243=EDGE_CURVE('',#8260,#8224,#1852,.T.);
#10244=EDGE_CURVE('',#8263,#8261,#1383,.T.);
#10245=EDGE_CURVE('',#8264,#8263,#1853,.T.);
#10246=EDGE_CURVE('',#8265,#8264,#1384,.T.);
#10247=EDGE_CURVE('',#8266,#8265,#1147,.F.);
#10248=EDGE_CURVE('',#8262,#8266,#1854,.T.);
#10249=EDGE_CURVE('',#8267,#8268,#7314,.T.);
#10250=EDGE_CURVE('',#8268,#8269,#99,.T.);
#10251=EDGE_CURVE('',#8269,#8270,#7315,.T.);
#10252=EDGE_CURVE('',#8270,#8271,#100,.T.);
#10253=EDGE_CURVE('',#8271,#8272,#7316,.T.);
#10254=EDGE_CURVE('',#8272,#8273,#101,.T.);
#10255=EDGE_CURVE('',#8273,#8274,#7317,.T.);
#10256=EDGE_CURVE('',#8274,#8275,#102,.T.);
#10257=EDGE_CURVE('',#8275,#8276,#7318,.T.);
#10258=EDGE_CURVE('',#8276,#8241,#1855,.T.);
#10259=EDGE_CURVE('',#8277,#8240,#103,.T.);
#10260=EDGE_CURVE('',#8277,#8278,#104,.T.);
#10261=EDGE_CURVE('',#8278,#8242,#105,.T.);
#10262=EDGE_CURVE('',#8276,#8279,#7319,.T.);
#10263=EDGE_CURVE('',#8279,#8280,#106,.T.);
#10264=EDGE_CURVE('',#8280,#8281,#7320,.T.);
#10265=EDGE_CURVE('',#8281,#8282,#107,.T.);
#10266=EDGE_CURVE('',#8282,#8283,#7321,.T.);
#10267=EDGE_CURVE('',#8283,#8284,#108,.T.);
#10268=EDGE_CURVE('',#8284,#8285,#7322,.T.);
#10269=EDGE_CURVE('',#8285,#8267,#109,.T.);
#10270=EDGE_CURVE('',#8286,#8287,#1148,.T.);
#10271=EDGE_CURVE('',#8286,#8287,#1149,.F.);
#10272=EDGE_CURVE('',#8288,#8289,#1385,.T.);
#10273=EDGE_CURVE('',#8289,#8290,#7323,.T.);
#10274=EDGE_CURVE('',#8290,#8291,#1856,.T.);
#10275=EDGE_CURVE('',#8291,#8287,#7324,.T.);
#10276=EDGE_CURVE('',#8286,#8291,#7325,.T.);
#10277=EDGE_CURVE('',#8290,#8288,#7326,.T.);
#10278=EDGE_CURVE('',#8292,#8293,#7327,.T.);
#10279=EDGE_CURVE('',#8294,#8292,#1857,.T.);
#10280=EDGE_CURVE('',#8295,#8294,#7328,.T.);
#10281=EDGE_CURVE('',#8293,#8295,#1858,.T.);
#10282=EDGE_CURVE('',#8296,#8297,#7329,.T.);
#10283=EDGE_CURVE('',#8297,#8298,#1859,.T.);
#10284=EDGE_CURVE('',#8298,#8299,#7330,.T.);
#10285=EDGE_CURVE('',#8283,#8299,#1860,.T.);
#10286=EDGE_CURVE('',#8282,#8300,#1861,.T.);
#10287=EDGE_CURVE('',#8300,#8301,#7331,.T.);
#10288=EDGE_CURVE('',#8301,#8296,#1862,.T.);
#10289=EDGE_CURVE('',#8291,#8302,#1863,.T.);
#10290=EDGE_CURVE('',#8302,#8302,#7332,.T.);
#10291=EDGE_CURVE('',#8303,#8303,#7333,.T.);
#10292=EDGE_CURVE('',#8303,#8304,#1864,.T.);
#10293=EDGE_CURVE('',#8304,#8304,#7334,.T.);
#10294=EDGE_CURVE('',#8305,#8305,#7335,.T.);
#10295=EDGE_CURVE('',#8305,#8306,#1865,.T.);
#10296=EDGE_CURVE('',#8306,#8306,#7336,.T.);
#10297=EDGE_CURVE('',#8307,#8307,#7337,.T.);
#10298=EDGE_CURVE('',#8307,#8308,#1866,.T.);
#10299=EDGE_CURVE('',#8308,#8308,#7338,.T.);
#10300=EDGE_CURVE('',#8309,#8309,#7339,.T.);
#10301=EDGE_CURVE('',#8309,#8310,#1867,.T.);
#10302=EDGE_CURVE('',#8310,#8310,#7340,.T.);
#10303=EDGE_CURVE('',#8311,#8311,#7341,.T.);
#10304=EDGE_CURVE('',#8311,#8312,#1868,.T.);
#10305=EDGE_CURVE('',#8312,#8313,#7342,.T.);
#10306=EDGE_CURVE('',#8313,#8314,#1869,.T.);
#10307=EDGE_CURVE('',#8314,#8315,#7343,.T.);
#10308=EDGE_CURVE('',#8315,#8316,#1870,.T.);
#10309=EDGE_CURVE('',#8316,#8316,#7344,.T.);
#10310=EDGE_CURVE('',#8315,#8317,#7345,.T.);
#10311=EDGE_CURVE('',#8317,#8318,#1871,.T.);
#10312=EDGE_CURVE('',#8318,#8312,#7346,.T.);
#10313=EDGE_CURVE('',#8319,#8319,#7347,.T.);
#10314=EDGE_CURVE('',#8319,#8320,#1872,.T.);
#10315=EDGE_CURVE('',#8320,#8320,#7348,.T.);
#10316=EDGE_CURVE('',#8321,#8321,#7349,.T.);
#10317=EDGE_CURVE('',#8321,#8322,#1873,.T.);
#10318=EDGE_CURVE('',#8322,#8322,#7350,.T.);
#10319=EDGE_CURVE('',#8316,#8323,#1874,.T.);
#10320=EDGE_CURVE('',#8323,#8323,#7351,.T.);
#10321=EDGE_CURVE('',#8324,#8324,#7352,.T.);
#10322=EDGE_CURVE('',#8324,#8325,#1875,.T.);
#10323=EDGE_CURVE('',#8325,#8325,#7353,.T.);
#10324=EDGE_CURVE('',#8326,#8326,#7354,.T.);
#10325=EDGE_CURVE('',#8326,#8327,#1876,.T.);
#10326=EDGE_CURVE('',#8327,#8327,#7355,.T.);
#10327=EDGE_CURVE('',#8328,#8328,#7356,.T.);
#10328=EDGE_CURVE('',#8328,#8329,#1877,.T.);
#10329=EDGE_CURVE('',#8329,#8329,#7357,.T.);
#10330=EDGE_CURVE('',#8330,#8330,#7358,.T.);
#10331=EDGE_CURVE('',#8330,#8331,#1878,.T.);
#10332=EDGE_CURVE('',#8331,#8331,#7359,.T.);
#10333=EDGE_CURVE('',#8332,#8332,#7360,.T.);
#10334=EDGE_CURVE('',#8332,#8333,#1879,.T.);
#10335=EDGE_CURVE('',#8333,#8333,#7361,.T.);
#10336=EDGE_CURVE('',#8334,#8334,#7362,.T.);
#10337=EDGE_CURVE('',#8334,#8335,#1880,.T.);
#10338=EDGE_CURVE('',#8335,#8335,#7363,.T.);
#10339=EDGE_CURVE('',#8336,#8337,#7364,.T.);
#10340=EDGE_CURVE('',#8338,#8337,#1881,.T.);
#10341=EDGE_CURVE('',#8338,#8339,#7365,.T.);
#10342=EDGE_CURVE('',#8336,#8339,#1882,.T.);
#10343=EDGE_CURVE('',#8171,#8340,#1883,.T.);
#10344=EDGE_CURVE('',#8341,#8340,#7366,.T.);
#10345=EDGE_CURVE('',#8340,#8341,#7367,.T.);
#10346=EDGE_CURVE('',#8342,#8343,#7368,.T.);
#10347=EDGE_CURVE('',#8344,#8343,#1884,.T.);
#10348=EDGE_CURVE('',#8345,#8344,#7369,.T.);
#10349=EDGE_CURVE('',#8345,#8342,#1885,.T.);
#10350=EDGE_CURVE('',#8346,#8347,#7370,.T.);
#10351=EDGE_CURVE('',#8347,#8346,#7371,.T.);
#10352=EDGE_CURVE('',#8347,#8341,#1886,.T.);
#10353=EDGE_CURVE('',#8348,#8349,#7372,.T.);
#10354=EDGE_CURVE('',#8349,#8348,#7373,.T.);
#10355=EDGE_CURVE('',#8349,#8346,#1887,.T.);
#10356=EDGE_CURVE('',#8350,#8351,#1150,.T.);
#10357=EDGE_CURVE('',#8351,#8352,#1151,.T.);
#10358=EDGE_CURVE('',#8352,#8353,#7374,.T.);
#10359=EDGE_CURVE('',#8353,#8354,#1152,.T.);
#10360=EDGE_CURVE('',#8354,#8355,#1153,.T.);
#10361=EDGE_CURVE('',#8355,#8356,#1154,.T.);
#10362=EDGE_CURVE('',#8356,#8357,#7375,.T.);
#10363=EDGE_CURVE('',#8357,#8358,#1155,.T.);
#10364=EDGE_CURVE('',#8358,#8359,#1156,.T.);
#10365=EDGE_CURVE('',#8360,#8359,#1888,.T.);
#10366=EDGE_CURVE('',#8361,#8360,#7376,.T.);
#10367=EDGE_CURVE('',#8361,#8362,#1889,.T.);
#10368=EDGE_CURVE('',#8362,#8363,#1157,.T.);
#10369=EDGE_CURVE('',#8363,#8364,#1158,.T.);
#10370=EDGE_CURVE('',#8364,#8365,#7377,.T.);
#10371=EDGE_CURVE('',#8365,#8366,#1159,.T.);
#10372=EDGE_CURVE('',#8366,#8367,#1160,.T.);
#10373=EDGE_CURVE('',#8367,#8368,#1161,.T.);
#10374=EDGE_CURVE('',#8368,#8369,#7378,.T.);
#10375=EDGE_CURVE('',#8369,#8350,#1162,.T.);
#10376=EDGE_CURVE('',#8370,#8370,#7379,.T.);
#10377=EDGE_CURVE('',#8370,#8371,#1890,.T.);
#10378=EDGE_CURVE('',#8371,#8371,#7380,.T.);
#10379=EDGE_CURVE('',#8372,#8372,#7381,.T.);
#10380=EDGE_CURVE('',#8372,#8373,#1891,.T.);
#10381=EDGE_CURVE('',#8373,#8373,#7382,.T.);
#10382=EDGE_CURVE('',#8348,#8374,#1892,.T.);
#10383=EDGE_CURVE('',#8374,#8374,#7383,.T.);
#10384=EDGE_CURVE('',#8375,#8375,#7384,.T.);
#10385=EDGE_CURVE('',#8375,#8376,#1893,.T.);
#10386=EDGE_CURVE('',#8377,#8376,#7385,.T.);
#10387=EDGE_CURVE('',#8376,#8377,#7386,.T.);
#10388=EDGE_CURVE('',#8378,#8379,#7387,.T.);
#10389=EDGE_CURVE('',#8378,#8380,#1894,.T.);
#10390=EDGE_CURVE('',#8381,#8380,#7388,.T.);
#10391=EDGE_CURVE('',#8379,#8381,#1895,.T.);
#10392=EDGE_CURVE('',#8382,#8377,#1896,.T.);
#10393=EDGE_CURVE('',#8383,#8384,#1386,.T.);
#10394=EDGE_CURVE('',#8384,#8383,#1163,.T.);
#10395=EDGE_CURVE('',#8165,#8359,#1387,.T.);
#10396=EDGE_CURVE('',#8359,#8165,#1164,.T.);
#10397=EDGE_CURVE('',#8359,#8385,#1897,.T.);
#10398=EDGE_CURVE('',#8386,#8385,#1165,.T.);
#10399=EDGE_CURVE('',#8386,#8166,#1166,.T.);
#10400=EDGE_CURVE('',#8387,#8388,#1898,.T.);
#10401=EDGE_CURVE('',#8388,#8387,#1167,.T.);
#10402=EDGE_CURVE('',#8389,#8390,#1899,.T.);
#10403=EDGE_CURVE('',#8391,#8389,#1168,.T.);
#10404=EDGE_CURVE('',#8392,#8391,#1169,.T.);
#10405=EDGE_CURVE('',#8392,#8366,#1900,.T.);
#10406=EDGE_CURVE('',#8364,#8365,#1170,.T.);
#10407=EDGE_CURVE('',#8390,#8363,#1171,.T.);
#10408=EDGE_CURVE('',#8362,#8393,#1388,.T.);
#10409=EDGE_CURVE('',#8393,#8362,#1172,.T.);
#10410=EDGE_CURVE('',#8362,#8394,#1901,.T.);
#10411=EDGE_CURVE('',#8393,#8395,#1902,.T.);
#10412=EDGE_CURVE('',#8395,#8396,#1173,.T.);
#10413=EDGE_CURVE('',#8394,#8396,#1174,.T.);
#10414=EDGE_CURVE('',#8397,#8398,#1389,.T.);
#10415=EDGE_CURVE('',#8398,#8397,#1175,.T.);
#10416=EDGE_CURVE('',#8397,#8399,#1903,.T.);
#10417=EDGE_CURVE('',#8398,#8400,#1904,.T.);
#10418=EDGE_CURVE('',#8401,#8400,#1176,.T.);
#10419=EDGE_CURVE('',#8401,#8399,#1177,.T.);
#10420=EDGE_CURVE('',#8402,#8403,#1390,.T.);
#10421=EDGE_CURVE('',#8403,#8402,#1178,.T.);
#10422=EDGE_CURVE('',#8404,#8405,#1391,.T.);
#10423=EDGE_CURVE('',#8405,#8404,#1179,.T.);
#10424=EDGE_CURVE('',#8406,#8407,#1905,.T.);
#10425=EDGE_CURVE('',#8408,#8406,#1906,.T.);
#10426=EDGE_CURVE('',#8409,#8408,#1907,.T.);
#10427=EDGE_CURVE('',#8410,#8409,#1908,.T.);
#10428=EDGE_CURVE('',#8411,#8410,#1909,.T.);
#10429=EDGE_CURVE('',#8407,#8411,#1910,.T.);
#10430=EDGE_CURVE('',#8412,#8413,#1911,.T.);
#10431=EDGE_CURVE('',#8414,#8412,#1912,.T.);
#10432=EDGE_CURVE('',#8415,#8414,#1913,.T.);
#10433=EDGE_CURVE('',#8416,#8415,#1914,.T.);
#10434=EDGE_CURVE('',#8417,#8416,#1915,.T.);
#10435=EDGE_CURVE('',#8413,#8417,#1916,.T.);
#10436=EDGE_CURVE('',#8418,#8419,#1917,.T.);
#10437=EDGE_CURVE('',#8420,#8418,#1918,.T.);
#10438=EDGE_CURVE('',#8421,#8420,#1919,.T.);
#10439=EDGE_CURVE('',#8422,#8421,#1920,.T.);
#10440=EDGE_CURVE('',#8423,#8422,#1921,.T.);
#10441=EDGE_CURVE('',#8419,#8423,#1922,.T.);
#10442=EDGE_CURVE('',#8424,#8425,#1923,.T.);
#10443=EDGE_CURVE('',#8426,#8424,#1924,.T.);
#10444=EDGE_CURVE('',#8427,#8426,#1925,.T.);
#10445=EDGE_CURVE('',#8428,#8427,#1926,.T.);
#10446=EDGE_CURVE('',#8429,#8428,#1927,.T.);
#10447=EDGE_CURVE('',#8425,#8429,#1928,.T.);
#10448=EDGE_CURVE('',#8430,#8431,#7389,.T.);
#10449=EDGE_CURVE('',#8431,#8432,#1929,.T.);
#10450=EDGE_CURVE('',#8432,#8433,#7390,.T.);
#10451=EDGE_CURVE('',#8433,#8434,#7391,.T.);
#10452=EDGE_CURVE('',#8434,#8435,#7392,.T.);
#10453=EDGE_CURVE('',#8435,#8436,#1930,.T.);
#10454=EDGE_CURVE('',#8436,#8378,#7393,.T.);
#10455=EDGE_CURVE('',#8379,#8437,#7394,.T.);
#10456=EDGE_CURVE('',#8437,#8438,#1931,.T.);
#10457=EDGE_CURVE('',#8438,#8439,#7395,.T.);
#10458=EDGE_CURVE('',#8439,#8440,#7396,.T.);
#10459=EDGE_CURVE('',#8440,#8441,#7397,.T.);
#10460=EDGE_CURVE('',#8441,#8442,#1932,.T.);
#10461=EDGE_CURVE('',#8442,#8443,#7398,.T.);
#10462=EDGE_CURVE('',#8443,#8430,#7399,.T.);
#10463=EDGE_CURVE('',#8444,#8445,#1933,.T.);
#10464=EDGE_CURVE('',#8445,#8446,#1934,.T.);
#10465=EDGE_CURVE('',#8446,#8447,#1935,.T.);
#10466=EDGE_CURVE('',#8447,#8448,#1936,.T.);
#10467=EDGE_CURVE('',#8448,#8449,#1937,.T.);
#10468=EDGE_CURVE('',#8449,#8444,#1938,.T.);
#10469=EDGE_CURVE('',#8450,#8451,#1939,.T.);
#10470=EDGE_CURVE('',#8451,#8452,#1940,.T.);
#10471=EDGE_CURVE('',#8452,#8453,#1941,.T.);
#10472=EDGE_CURVE('',#8453,#8454,#1942,.T.);
#10473=EDGE_CURVE('',#8454,#8455,#1943,.T.);
#10474=EDGE_CURVE('',#8455,#8450,#1944,.T.);
#10475=EDGE_CURVE('',#8456,#8457,#1945,.T.);
#10476=EDGE_CURVE('',#8410,#8457,#1946,.T.);
#10477=EDGE_CURVE('',#8456,#8409,#1947,.T.);
#10478=EDGE_CURVE('',#8457,#8458,#1948,.T.);
#10479=EDGE_CURVE('',#8411,#8458,#1949,.T.);
#10480=EDGE_CURVE('',#8458,#8459,#1950,.T.);
#10481=EDGE_CURVE('',#8407,#8459,#1951,.T.);
#10482=EDGE_CURVE('',#8459,#8460,#1952,.T.);
#10483=EDGE_CURVE('',#8406,#8460,#1953,.T.);
#10484=EDGE_CURVE('',#8460,#8461,#1954,.T.);
#10485=EDGE_CURVE('',#8408,#8461,#1955,.T.);
#10486=EDGE_CURVE('',#8461,#8456,#1956,.T.);
#10487=EDGE_CURVE('',#8462,#8463,#1957,.T.);
#10488=EDGE_CURVE('',#8462,#8464,#1958,.T.);
#10489=EDGE_CURVE('',#8464,#8465,#1959,.T.);
#10490=EDGE_CURVE('',#8466,#8465,#1960,.T.);
#10491=EDGE_CURVE('',#8463,#8466,#7400,.T.);
#10492=EDGE_CURVE('',#8467,#8468,#1961,.T.);
#10493=EDGE_CURVE('',#8465,#8468,#7401,.T.);
#10494=EDGE_CURVE('',#8464,#8467,#7402,.T.);
#10495=EDGE_CURVE('',#8468,#8469,#1962,.T.);
#10496=EDGE_CURVE('',#8467,#8470,#1963,.T.);
#10497=EDGE_CURVE('',#8471,#8470,#1964,.T.);
#10498=EDGE_CURVE('',#8469,#8471,#7403,.T.);
#10499=EDGE_CURVE('',#8472,#8473,#1965,.T.);
#10500=EDGE_CURVE('',#8415,#8472,#1966,.T.);
#10501=EDGE_CURVE('',#8473,#8414,#1967,.T.);
#10502=EDGE_CURVE('',#8473,#8474,#1968,.T.);
#10503=EDGE_CURVE('',#8474,#8412,#1969,.T.);
#10504=EDGE_CURVE('',#8474,#8475,#1970,.T.);
#10505=EDGE_CURVE('',#8475,#8413,#1971,.T.);
#10506=EDGE_CURVE('',#8475,#8476,#1972,.T.);
#10507=EDGE_CURVE('',#8476,#8417,#1973,.T.);
#10508=EDGE_CURVE('',#8476,#8477,#1974,.T.);
#10509=EDGE_CURVE('',#8477,#8416,#1975,.T.);
#10510=EDGE_CURVE('',#8477,#8472,#1976,.T.);
#10511=EDGE_CURVE('',#8478,#8479,#1977,.T.);
#10512=EDGE_CURVE('',#8478,#8480,#1978,.T.);
#10513=EDGE_CURVE('',#8481,#8480,#1979,.T.);
#10514=EDGE_CURVE('',#8482,#8481,#1980,.T.);
#10515=EDGE_CURVE('',#8479,#8482,#7404,.T.);
#10516=EDGE_CURVE('',#8483,#8484,#1981,.T.);
#10517=EDGE_CURVE('',#8480,#8484,#7405,.T.);
#10518=EDGE_CURVE('',#8483,#8478,#7406,.T.);
#10519=EDGE_CURVE('',#8485,#8486,#1982,.T.);
#10520=EDGE_CURVE('',#8484,#8485,#1983,.T.);
#10521=EDGE_CURVE('',#8487,#8483,#1984,.T.);
#10522=EDGE_CURVE('',#8486,#8487,#7407,.T.);
#10523=EDGE_CURVE('',#8488,#8489,#1985,.T.);
#10524=EDGE_CURVE('',#8421,#8488,#1986,.T.);
#10525=EDGE_CURVE('',#8489,#8420,#1987,.T.);
#10526=EDGE_CURVE('',#8489,#8490,#1988,.T.);
#10527=EDGE_CURVE('',#8490,#8418,#1989,.T.);
#10528=EDGE_CURVE('',#8490,#8491,#1990,.T.);
#10529=EDGE_CURVE('',#8491,#8419,#1991,.T.);
#10530=EDGE_CURVE('',#8491,#8492,#1992,.T.);
#10531=EDGE_CURVE('',#8492,#8423,#1993,.T.);
#10532=EDGE_CURVE('',#8492,#8493,#1994,.T.);
#10533=EDGE_CURVE('',#8493,#8422,#1995,.T.);
#10534=EDGE_CURVE('',#8493,#8488,#1996,.T.);
#10535=EDGE_CURVE('',#8494,#8495,#1997,.T.);
#10536=EDGE_CURVE('',#8494,#8496,#1998,.T.);
#10537=EDGE_CURVE('',#8497,#8496,#1999,.T.);
#10538=EDGE_CURVE('',#8498,#8497,#2000,.T.);
#10539=EDGE_CURVE('',#8495,#8498,#7408,.T.);
#10540=EDGE_CURVE('',#8499,#8500,#2001,.T.);
#10541=EDGE_CURVE('',#8496,#8500,#7409,.T.);
#10542=EDGE_CURVE('',#8499,#8494,#7410,.T.);
#10543=EDGE_CURVE('',#8501,#8502,#2002,.T.);
#10544=EDGE_CURVE('',#8500,#8501,#2003,.T.);
#10545=EDGE_CURVE('',#8503,#8499,#2004,.T.);
#10546=EDGE_CURVE('',#8502,#8503,#7411,.T.);
#10547=EDGE_CURVE('',#8487,#8469,#2005,.T.);
#10548=EDGE_CURVE('',#8504,#8479,#2006,.T.);
#10549=EDGE_CURVE('',#8504,#8505,#2007,.T.);
#10550=EDGE_CURVE('',#8505,#8506,#7412,.T.);
#10551=EDGE_CURVE('',#8506,#8507,#2008,.T.);
#10552=EDGE_CURVE('',#8503,#8507,#2009,.T.);
#10553=EDGE_CURVE('',#8466,#8495,#2010,.T.);
#10554=EDGE_CURVE('',#8508,#8509,#2011,.T.);
#10555=EDGE_CURVE('',#8427,#8508,#2012,.T.);
#10556=EDGE_CURVE('',#8509,#8426,#2013,.T.);
#10557=EDGE_CURVE('',#8509,#8510,#2014,.T.);
#10558=EDGE_CURVE('',#8510,#8424,#2015,.T.);
#10559=EDGE_CURVE('',#8510,#8511,#2016,.T.);
#10560=EDGE_CURVE('',#8511,#8425,#2017,.T.);
#10561=EDGE_CURVE('',#8511,#8512,#2018,.T.);
#10562=EDGE_CURVE('',#8512,#8429,#2019,.T.);
#10563=EDGE_CURVE('',#8512,#8513,#2020,.T.);
#10564=EDGE_CURVE('',#8513,#8428,#2021,.T.);
#10565=EDGE_CURVE('',#8513,#8508,#2022,.T.);
#10566=EDGE_CURVE('',#8506,#8514,#2023,.T.);
#10567=EDGE_CURVE('',#8515,#8514,#2024,.T.);
#10568=EDGE_CURVE('',#8516,#8515,#2025,.T.);
#10569=EDGE_CURVE('',#8507,#8516,#7413,.T.);
#10570=EDGE_CURVE('',#8505,#8517,#2026,.T.);
#10571=EDGE_CURVE('',#8514,#8517,#7414,.T.);
#10572=EDGE_CURVE('',#8518,#8519,#2027,.T.);
#10573=EDGE_CURVE('',#8517,#8518,#2028,.T.);
#10574=EDGE_CURVE('',#8519,#8504,#7415,.T.);
#10575=EDGE_CURVE('',#8520,#8433,#2029,.T.);
#10576=EDGE_CURVE('',#8432,#8521,#2030,.T.);
#10577=EDGE_CURVE('',#8520,#8521,#7416,.T.);
#10578=EDGE_CURVE('',#8431,#8522,#2031,.T.);
#10579=EDGE_CURVE('',#8521,#8522,#2032,.T.);
#10580=EDGE_CURVE('',#8430,#8523,#2033,.T.);
#10581=EDGE_CURVE('',#8522,#8523,#7417,.T.);
#10582=EDGE_CURVE('',#8443,#8524,#2034,.T.);
#10583=EDGE_CURVE('',#8523,#8524,#7418,.T.);
#10584=EDGE_CURVE('',#8442,#8525,#2035,.T.);
#10585=EDGE_CURVE('',#8524,#8525,#7419,.T.);
#10586=EDGE_CURVE('',#8441,#8526,#2036,.T.);
#10587=EDGE_CURVE('',#8525,#8526,#2037,.T.);
#10588=EDGE_CURVE('',#8440,#8527,#2038,.T.);
#10589=EDGE_CURVE('',#8526,#8527,#7420,.T.);
#10590=EDGE_CURVE('',#8439,#8528,#2039,.T.);
#10591=EDGE_CURVE('',#8527,#8528,#7421,.T.);
#10592=EDGE_CURVE('',#8438,#8529,#2040,.T.);
#10593=EDGE_CURVE('',#8528,#8529,#7422,.T.);
#10594=EDGE_CURVE('',#8437,#8530,#2041,.T.);
#10595=EDGE_CURVE('',#8529,#8530,#2042,.T.);
#10596=EDGE_CURVE('',#8530,#8381,#7423,.T.);
#10597=EDGE_CURVE('',#8436,#8531,#2043,.T.);
#10598=EDGE_CURVE('',#8380,#8531,#7424,.T.);
#10599=EDGE_CURVE('',#8435,#8532,#2044,.T.);
#10600=EDGE_CURVE('',#8531,#8532,#2045,.T.);
#10601=EDGE_CURVE('',#8434,#8533,#2046,.T.);
#10602=EDGE_CURVE('',#8532,#8533,#7425,.T.);
#10603=EDGE_CURVE('',#8533,#8520,#7426,.T.);
#10604=EDGE_CURVE('',#8534,#8446,#2047,.T.);
#10605=EDGE_CURVE('',#8445,#8535,#2048,.T.);
#10606=EDGE_CURVE('',#8534,#8535,#7427,.T.);
#10607=EDGE_CURVE('',#8444,#8536,#2049,.T.);
#10608=EDGE_CURVE('',#8535,#8536,#7428,.T.);
#10609=EDGE_CURVE('',#8449,#8537,#2050,.T.);
#10610=EDGE_CURVE('',#8536,#8537,#7429,.T.);
#10611=EDGE_CURVE('',#8448,#8538,#2051,.T.);
#10612=EDGE_CURVE('',#8537,#8538,#7430,.T.);
#10613=EDGE_CURVE('',#8447,#8539,#2052,.T.);
#10614=EDGE_CURVE('',#8538,#8539,#7431,.T.);
#10615=EDGE_CURVE('',#8539,#8534,#7432,.T.);
#10616=EDGE_CURVE('',#8540,#8452,#2053,.T.);
#10617=EDGE_CURVE('',#8451,#8541,#2054,.T.);
#10618=EDGE_CURVE('',#8540,#8541,#7433,.T.);
#10619=EDGE_CURVE('',#8450,#8542,#2055,.T.);
#10620=EDGE_CURVE('',#8541,#8542,#7434,.T.);
#10621=EDGE_CURVE('',#8455,#8543,#2056,.T.);
#10622=EDGE_CURVE('',#8542,#8543,#7435,.T.);
#10623=EDGE_CURVE('',#8454,#8544,#2057,.T.);
#10624=EDGE_CURVE('',#8543,#8544,#7436,.T.);
#10625=EDGE_CURVE('',#8453,#8545,#2058,.T.);
#10626=EDGE_CURVE('',#8544,#8545,#7437,.T.);
#10627=EDGE_CURVE('',#8545,#8540,#7438,.T.);
#10628=EDGE_CURVE('',#8463,#8498,#2059,.T.);
#10629=EDGE_CURVE('',#8486,#8471,#2060,.T.);
#10630=EDGE_CURVE('',#8546,#8547,#7439,.T.);
#10631=EDGE_CURVE('',#8470,#8546,#2061,.T.);
#10632=EDGE_CURVE('',#8547,#8462,#2062,.T.);
#10633=EDGE_CURVE('',#8519,#8482,#2063,.T.);
#10634=EDGE_CURVE('',#8548,#8485,#2064,.T.);
#10635=EDGE_CURVE('',#8549,#8548,#7440,.T.);
#10636=EDGE_CURVE('',#8481,#8549,#2065,.T.);
#10637=EDGE_CURVE('',#8550,#8501,#2066,.T.);
#10638=EDGE_CURVE('',#8551,#8550,#7441,.T.);
#10639=EDGE_CURVE('',#8497,#8551,#2067,.T.);
#10640=EDGE_CURVE('',#8502,#8516,#2068,.T.);
#10641=EDGE_CURVE('',#8552,#8518,#2069,.T.);
#10642=EDGE_CURVE('',#8553,#8552,#7442,.T.);
#10643=EDGE_CURVE('',#8515,#8553,#2070,.T.);
#10644=EDGE_CURVE('',#8554,#8555,#1180,.T.);
#10645=EDGE_CURVE('',#8556,#8554,#2071,.T.);
#10646=EDGE_CURVE('',#8557,#8556,#2072,.T.);
#10647=EDGE_CURVE('',#8555,#8557,#1181,.T.);
#10648=EDGE_CURVE('',#8558,#8556,#7443,.T.);
#10649=EDGE_CURVE('',#8559,#8558,#2073,.T.);
#10650=EDGE_CURVE('',#8557,#8559,#1182,.T.);
#10651=EDGE_CURVE('',#8560,#8558,#2074,.T.);
#10652=EDGE_CURVE('',#8561,#8560,#1183,.T.);
#10653=EDGE_CURVE('',#8559,#8561,#1184,.T.);
#10654=EDGE_CURVE('',#8562,#8401,#2075,.T.);
#10655=EDGE_CURVE('',#8563,#8562,#2076,.T.);
#10656=EDGE_CURVE('',#8399,#8563,#1185,.T.);
#10657=EDGE_CURVE('',#8564,#8562,#7444,.T.);
#10658=EDGE_CURVE('',#8565,#8564,#2077,.T.);
#10659=EDGE_CURVE('',#8563,#8565,#1186,.T.);
#10660=EDGE_CURVE('',#8565,#8395,#1187,.T.);
#10661=EDGE_CURVE('',#8396,#8564,#2078,.T.);
#10662=EDGE_CURVE('',#8566,#8386,#2079,.T.);
#10663=EDGE_CURVE('',#8167,#8566,#2080,.T.);
#10664=EDGE_CURVE('',#8567,#8566,#7445,.T.);
#10665=EDGE_CURVE('',#8168,#8567,#2081,.T.);
#10666=EDGE_CURVE('',#8163,#8567,#2082,.T.);
#10667=EDGE_CURVE('',#8568,#8569,#1188,.T.);
#10668=EDGE_CURVE('',#8570,#8569,#2083,.T.);
#10669=EDGE_CURVE('',#8571,#8570,#2084,.T.);
#10670=EDGE_CURVE('',#8568,#8571,#1189,.T.);
#10671=EDGE_CURVE('',#8572,#8570,#7446,.T.);
#10672=EDGE_CURVE('',#8573,#8572,#2085,.T.);
#10673=EDGE_CURVE('',#8571,#8573,#1190,.T.);
#10674=EDGE_CURVE('',#8573,#8574,#1191,.T.);
#10675=EDGE_CURVE('',#8575,#8572,#2086,.T.);
#10676=EDGE_CURVE('',#8574,#8575,#1192,.T.);
#10677=EDGE_CURVE('',#8576,#8577,#1193,.T.);
#10678=EDGE_CURVE('',#8164,#8577,#110,.T.);
#10679=EDGE_CURVE('',#8385,#8386,#1194,.T.);
#10680=EDGE_CURVE('',#8578,#8385,#7447,.T.);
#10681=EDGE_CURVE('',#8578,#8579,#1195,.T.);
#10682=EDGE_CURVE('',#8579,#8580,#1196,.T.);
#10683=EDGE_CURVE('',#8580,#8581,#1197,.T.);
#10684=EDGE_CURVE('',#8581,#8582,#1198,.T.);
#10685=EDGE_CURVE('',#8582,#8583,#1199,.T.);
#10686=EDGE_CURVE('',#8583,#8392,#1200,.T.);
#10687=EDGE_CURVE('',#8394,#8391,#7448,.T.);
#10688=EDGE_CURVE('',#8396,#8394,#1201,.T.);
#10689=EDGE_CURVE('',#8400,#8401,#1202,.T.);
#10690=EDGE_CURVE('',#8584,#8400,#7449,.T.);
#10691=EDGE_CURVE('',#8584,#8585,#1203,.T.);
#10692=EDGE_CURVE('',#8585,#8586,#1204,.T.);
#10693=EDGE_CURVE('',#8586,#8587,#1205,.T.);
#10694=EDGE_CURVE('',#8587,#8588,#1206,.T.);
#10695=EDGE_CURVE('',#8588,#8589,#1207,.T.);
#10696=EDGE_CURVE('',#8589,#8590,#1208,.T.);
#10697=EDGE_CURVE('',#8590,#8591,#1209,.T.);
#10698=EDGE_CURVE('',#8592,#8591,#7450,.T.);
#10699=EDGE_CURVE('',#8560,#8592,#111,.T.);
#10700=EDGE_CURVE('',#8593,#8554,#112,.T.);
#10701=EDGE_CURVE('',#8594,#8593,#7451,.T.);
#10702=EDGE_CURVE('',#8594,#8595,#1210,.T.);
#10703=EDGE_CURVE('',#8595,#8596,#1211,.T.);
#10704=EDGE_CURVE('',#8596,#8597,#1212,.T.);
#10705=EDGE_CURVE('',#8597,#8598,#1213,.T.);
#10706=EDGE_CURVE('',#8598,#8599,#1214,.T.);
#10707=EDGE_CURVE('',#8599,#8600,#1215,.T.);
#10708=EDGE_CURVE('',#8600,#8601,#1216,.T.);
#10709=EDGE_CURVE('',#8602,#8601,#7452,.T.);
#10710=EDGE_CURVE('',#8575,#8602,#1217,.T.);
#10711=EDGE_CURVE('',#8569,#8603,#1218,.T.);
#10712=EDGE_CURVE('',#8604,#8603,#7453,.T.);
#10713=EDGE_CURVE('',#8604,#8605,#1219,.T.);
#10714=EDGE_CURVE('',#8605,#8606,#1220,.T.);
#10715=EDGE_CURVE('',#8606,#8607,#1221,.T.);
#10716=EDGE_CURVE('',#8607,#8608,#1222,.T.);
#10717=EDGE_CURVE('',#8608,#8609,#1223,.T.);
#10718=EDGE_CURVE('',#8609,#8576,#1224,.T.);
#10719=EDGE_CURVE('',#8610,#8611,#7454,.T.);
#10720=EDGE_CURVE('',#8551,#8611,#2087,.T.);
#10721=EDGE_CURVE('',#8610,#8550,#2088,.T.);
#10722=EDGE_CURVE('',#8611,#8612,#2089,.T.);
#10723=EDGE_CURVE('',#8547,#8612,#2090,.T.);
#10724=EDGE_CURVE('',#8612,#8613,#7455,.T.);
#10725=EDGE_CURVE('',#8546,#8613,#2091,.T.);
#10726=EDGE_CURVE('',#8613,#8614,#2092,.T.);
#10727=EDGE_CURVE('',#8548,#8614,#2093,.T.);
#10728=EDGE_CURVE('',#8614,#8615,#7456,.T.);
#10729=EDGE_CURVE('',#8549,#8615,#2094,.T.);
#10730=EDGE_CURVE('',#8615,#8616,#2095,.T.);
#10731=EDGE_CURVE('',#8552,#8616,#2096,.T.);
#10732=EDGE_CURVE('',#8616,#8617,#7457,.T.);
#10733=EDGE_CURVE('',#8553,#8617,#2097,.T.);
#10734=EDGE_CURVE('',#8617,#8610,#2098,.T.);
#10735=EDGE_CURVE('',#8404,#8555,#2099,.T.);
#10736=EDGE_CURVE('',#8593,#8405,#2100,.T.);
#10737=EDGE_CURVE('',#8403,#8561,#2101,.T.);
#10738=EDGE_CURVE('',#8404,#8403,#1225,.T.);
#10739=EDGE_CURVE('',#8402,#8592,#2102,.T.);
#10740=EDGE_CURVE('',#8591,#8618,#1226,.T.);
#10741=EDGE_CURVE('',#8402,#8618,#1227,.T.);
#10742=EDGE_CURVE('',#8619,#8620,#7458,.T.);
#10743=EDGE_CURVE('',#8619,#8620,#1228,.T.);
#10744=EDGE_CURVE('',#8618,#8619,#1229,.T.);
#10745=EDGE_CURVE('',#8590,#8621,#2103,.T.);
#10746=EDGE_CURVE('',#8620,#8621,#1230,.T.);
#10747=EDGE_CURVE('',#8589,#8622,#2104,.T.);
#10748=EDGE_CURVE('',#8621,#8622,#1231,.T.);
#10749=EDGE_CURVE('',#8623,#8624,#7459,.T.);
#10750=EDGE_CURVE('',#8623,#8624,#1232,.T.);
#10751=EDGE_CURVE('',#8588,#8625,#2105,.T.);
#10752=EDGE_CURVE('',#8624,#8625,#1233,.T.);
#10753=EDGE_CURVE('',#8622,#8623,#1234,.T.);
#10754=EDGE_CURVE('',#8587,#8626,#2106,.T.);
#10755=EDGE_CURVE('',#8625,#8626,#1235,.F.);
#10756=EDGE_CURVE('',#8627,#8628,#7460,.T.);
#10757=EDGE_CURVE('',#8627,#8628,#1236,.T.);
#10758=EDGE_CURVE('',#8586,#8629,#2107,.T.);
#10759=EDGE_CURVE('',#8628,#8629,#1237,.T.);
#10760=EDGE_CURVE('',#8626,#8627,#1238,.T.);
#10761=EDGE_CURVE('',#8585,#8630,#2108,.T.);
#10762=EDGE_CURVE('',#8629,#8630,#1239,.T.);
#10763=EDGE_CURVE('',#8631,#8632,#7461,.T.);
#10764=EDGE_CURVE('',#8631,#8632,#1240,.T.);
#10765=EDGE_CURVE('',#8633,#8584,#1241,.T.);
#10766=EDGE_CURVE('',#8632,#8633,#1242,.T.);
#10767=EDGE_CURVE('',#8630,#8631,#1243,.T.);
#10768=EDGE_CURVE('',#8633,#8398,#1244,.T.);
#10769=EDGE_CURVE('',#8397,#8393,#1245,.T.);
#10770=EDGE_CURVE('',#8356,#8357,#1246,.T.);
#10771=EDGE_CURVE('',#8358,#8388,#1247,.T.);
#10772=EDGE_CURVE('',#8387,#8578,#1248,.T.);
#10773=EDGE_CURVE('',#8389,#8390,#7462,.T.);
#10774=EDGE_CURVE('',#8583,#8367,#2109,.T.);
#10775=EDGE_CURVE('',#8368,#8369,#1249,.T.);
#10776=EDGE_CURVE('',#8582,#8350,#2110,.T.);
#10777=EDGE_CURVE('',#8581,#8351,#2111,.T.);
#10778=EDGE_CURVE('',#8352,#8353,#1250,.T.);
#10779=EDGE_CURVE('',#8580,#8354,#2112,.T.);
#10780=EDGE_CURVE('',#8579,#8355,#2113,.T.);
#10781=EDGE_CURVE('',#8165,#8160,#1251,.T.);
#10782=EDGE_CURVE('',#8160,#8161,#1252,.T.);
#10783=EDGE_CURVE('',#8577,#8634,#1253,.T.);
#10784=EDGE_CURVE('',#8161,#8634,#1254,.T.);
#10785=EDGE_CURVE('',#8635,#8636,#7463,.T.);
#10786=EDGE_CURVE('',#8635,#8636,#1255,.T.);
#10787=EDGE_CURVE('',#8634,#8635,#1256,.T.);
#10788=EDGE_CURVE('',#8576,#8637,#2114,.T.);
#10789=EDGE_CURVE('',#8636,#8637,#1257,.T.);
#10790=EDGE_CURVE('',#8609,#8638,#2115,.T.);
#10791=EDGE_CURVE('',#8637,#8638,#1258,.T.);
#10792=EDGE_CURVE('',#8639,#8640,#7464,.T.);
#10793=EDGE_CURVE('',#8639,#8640,#1259,.T.);
#10794=EDGE_CURVE('',#8608,#8641,#2116,.T.);
#10795=EDGE_CURVE('',#8640,#8641,#1260,.T.);
#10796=EDGE_CURVE('',#8638,#8639,#1261,.T.);
#10797=EDGE_CURVE('',#8607,#8642,#2117,.T.);
#10798=EDGE_CURVE('',#8641,#8642,#1262,.T.);
#10799=EDGE_CURVE('',#8643,#8644,#7465,.T.);
#10800=EDGE_CURVE('',#8643,#8644,#1263,.T.);
#10801=EDGE_CURVE('',#8606,#8645,#2118,.T.);
#10802=EDGE_CURVE('',#8644,#8645,#1264,.T.);
#10803=EDGE_CURVE('',#8642,#8643,#1265,.T.);
#10804=EDGE_CURVE('',#8605,#8646,#2119,.T.);
#10805=EDGE_CURVE('',#8645,#8646,#1266,.T.);
#10806=EDGE_CURVE('',#8647,#8648,#7466,.T.);
#10807=EDGE_CURVE('',#8647,#8648,#1267,.T.);
#10808=EDGE_CURVE('',#8649,#8604,#1268,.T.);
#10809=EDGE_CURVE('',#8648,#8649,#1269,.T.);
#10810=EDGE_CURVE('',#8646,#8647,#1270,.T.);
#10811=EDGE_CURVE('',#8603,#8650,#1271,.T.);
#10812=EDGE_CURVE('',#8649,#8650,#1272,.T.);
#10813=EDGE_CURVE('',#8651,#8568,#1273,.T.);
#10814=EDGE_CURVE('',#8650,#8651,#1274,.T.);
#10815=EDGE_CURVE('',#8652,#8574,#2120,.T.);
#10816=EDGE_CURVE('',#8651,#8652,#1275,.T.);
#10817=EDGE_CURVE('',#8383,#8602,#2121,.T.);
#10818=EDGE_CURVE('',#8652,#8384,#7467,.T.);
#10819=EDGE_CURVE('',#8653,#8654,#7468,.T.);
#10820=EDGE_CURVE('',#8653,#8654,#1276,.T.);
#10821=EDGE_CURVE('',#8655,#8405,#1277,.T.);
#10822=EDGE_CURVE('',#8655,#8594,#1278,.T.);
#10823=EDGE_CURVE('',#8601,#8656,#1279,.T.);
#10824=EDGE_CURVE('',#8383,#8656,#1280,.T.);
#10825=EDGE_CURVE('',#8657,#8658,#7469,.T.);
#10826=EDGE_CURVE('',#8657,#8658,#7470,.T.);
#10827=EDGE_CURVE('',#8656,#8657,#1281,.T.);
#10828=EDGE_CURVE('',#8600,#8659,#2122,.T.);
#10829=EDGE_CURVE('',#8658,#8659,#1282,.T.);
#10830=EDGE_CURVE('',#8599,#8660,#2123,.T.);
#10831=EDGE_CURVE('',#8659,#8660,#1283,.T.);
#10832=EDGE_CURVE('',#8661,#8662,#7471,.T.);
#10833=EDGE_CURVE('',#8661,#8662,#1284,.T.);
#10834=EDGE_CURVE('',#8598,#8663,#2124,.T.);
#10835=EDGE_CURVE('',#8662,#8663,#1285,.T.);
#10836=EDGE_CURVE('',#8660,#8661,#1286,.T.);
#10837=EDGE_CURVE('',#8597,#8664,#2125,.T.);
#10838=EDGE_CURVE('',#8663,#8664,#1287,.T.);
#10839=EDGE_CURVE('',#8665,#8666,#7472,.T.);
#10840=EDGE_CURVE('',#8665,#8666,#1288,.T.);
#10841=EDGE_CURVE('',#8596,#8667,#2126,.T.);
#10842=EDGE_CURVE('',#8666,#8667,#1289,.T.);
#10843=EDGE_CURVE('',#8664,#8665,#1290,.T.);
#10844=EDGE_CURVE('',#8595,#8668,#2127,.T.);
#10845=EDGE_CURVE('',#8667,#8668,#1291,.T.);
#10846=EDGE_CURVE('',#8654,#8655,#1292,.T.);
#10847=EDGE_CURVE('',#8668,#8653,#1293,.T.);
#10848=EDGE_CURVE('',#8669,#8670,#2128,.T.);
#10849=EDGE_CURVE('',#8671,#8669,#7473,.T.);
#10850=EDGE_CURVE('',#8672,#8671,#2129,.T.);
#10851=EDGE_CURVE('',#8673,#8672,#7474,.T.);
#10852=EDGE_CURVE('',#8674,#8673,#2130,.T.);
#10853=EDGE_CURVE('',#8675,#8674,#7475,.T.);
#10854=EDGE_CURVE('',#8676,#8675,#2131,.T.);
#10855=EDGE_CURVE('',#8670,#8676,#7476,.T.);
#10856=EDGE_CURVE('',#8677,#8678,#7477,.T.);
#10857=EDGE_CURVE('',#8405,#8677,#2132,.T.);
#10858=EDGE_CURVE('',#8678,#8404,#2133,.T.);
#10859=EDGE_CURVE('',#8678,#8679,#7478,.T.);
#10860=EDGE_CURVE('',#8679,#8403,#2134,.T.);
#10861=EDGE_CURVE('',#8679,#8680,#7479,.T.);
#10862=EDGE_CURVE('',#8680,#8402,#2135,.T.);
#10863=EDGE_CURVE('',#8681,#8398,#2136,.T.);
#10864=EDGE_CURVE('',#8680,#8681,#7480,.T.);
#10865=EDGE_CURVE('',#8681,#8682,#7481,.T.);
#10866=EDGE_CURVE('',#8682,#8397,#2137,.T.);
#10867=EDGE_CURVE('',#8682,#8683,#7482,.T.);
#10868=EDGE_CURVE('',#8683,#8393,#2138,.T.);
#10869=EDGE_CURVE('',#8683,#8361,#7483,.T.);
#10870=EDGE_CURVE('',#8360,#8684,#7484,.T.);
#10871=EDGE_CURVE('',#8684,#8165,#2139,.T.);
#10872=EDGE_CURVE('',#8684,#8685,#7485,.T.);
#10873=EDGE_CURVE('',#8685,#8160,#2140,.T.);
#10874=EDGE_CURVE('',#8685,#8686,#7486,.T.);
#10875=EDGE_CURVE('',#8686,#8161,#1294,.T.);
#10876=EDGE_CURVE('',#8687,#8650,#2141,.T.);
#10877=EDGE_CURVE('',#8686,#8687,#7487,.T.);
#10878=EDGE_CURVE('',#8687,#8688,#7488,.T.);
#10879=EDGE_CURVE('',#8688,#8651,#2142,.T.);
#10880=EDGE_CURVE('',#8688,#8689,#7489,.T.);
#10881=EDGE_CURVE('',#8689,#8652,#2143,.T.);
#10882=EDGE_CURVE('',#8689,#8690,#7490,.T.);
#10883=EDGE_CURVE('',#8690,#8383,#2144,.T.);
#10884=EDGE_CURVE('',#8690,#8677,#7491,.T.);
#10885=EDGE_CURVE('',#8674,#8691,#2145,.T.);
#10886=EDGE_CURVE('',#8692,#8673,#2146,.T.);
#10887=EDGE_CURVE('',#8691,#8692,#2147,.T.);
#10888=EDGE_CURVE('',#8676,#8693,#2148,.T.);
#10889=EDGE_CURVE('',#8694,#8675,#2149,.T.);
#10890=EDGE_CURVE('',#8693,#8694,#2150,.T.);
#10891=EDGE_CURVE('',#8695,#8691,#1295,.T.);
#10892=EDGE_CURVE('',#8695,#8696,#7492,.T.);
#10893=EDGE_CURVE('',#8694,#8696,#1296,.T.);
#10894=EDGE_CURVE('',#8669,#8697,#2151,.T.);
#10895=EDGE_CURVE('',#8698,#8670,#2152,.T.);
#10896=EDGE_CURVE('',#8697,#8698,#2153,.T.);
#10897=EDGE_CURVE('',#8699,#8693,#1297,.T.);
#10898=EDGE_CURVE('',#8699,#8700,#7493,.T.);
#10899=EDGE_CURVE('',#8698,#8700,#1298,.T.);
#10900=EDGE_CURVE('',#8701,#8697,#1299,.T.);
#10901=EDGE_CURVE('',#8701,#8702,#7494,.T.);
#10902=EDGE_CURVE('',#8703,#8702,#1300,.T.);
#10903=EDGE_CURVE('',#8671,#8703,#2154,.T.);
#10904=EDGE_CURVE('',#8704,#8672,#2155,.T.);
#10905=EDGE_CURVE('',#8705,#8704,#1301,.T.);
#10906=EDGE_CURVE('',#8705,#8706,#7495,.T.);
#10907=EDGE_CURVE('',#8692,#8706,#1302,.T.);
#10908=EDGE_CURVE('',#8704,#8703,#2156,.T.);
#10909=EDGE_CURVE('',#8707,#8708,#1303,.T.);
#10910=EDGE_CURVE('',#8707,#8709,#2157,.T.);
#10911=EDGE_CURVE('',#8710,#8709,#7496,.T.);
#10912=EDGE_CURVE('',#8708,#8710,#1304,.T.);
#10913=EDGE_CURVE('',#8711,#8707,#1392,.T.);
#10914=EDGE_CURVE('',#8711,#8712,#2158,.T.);
#10915=EDGE_CURVE('',#8709,#8712,#1305,.T.);
#10916=EDGE_CURVE('',#8713,#8711,#1306,.T.);
#10917=EDGE_CURVE('',#8714,#8713,#1307,.T.);
#10918=EDGE_CURVE('',#8712,#8714,#7497,.T.);
#10919=EDGE_CURVE('',#8715,#8716,#2159,.T.);
#10920=EDGE_CURVE('',#8715,#8717,#7498,.T.);
#10921=EDGE_CURVE('',#8718,#8717,#1308,.T.);
#10922=EDGE_CURVE('',#8716,#8718,#1309,.T.);
#10923=EDGE_CURVE('',#8719,#8720,#2160,.T.);
#10924=EDGE_CURVE('',#8715,#8719,#1310,.T.);
#10925=EDGE_CURVE('',#8720,#8716,#1393,.T.);
#10926=EDGE_CURVE('',#8721,#8720,#1311,.T.);
#10927=EDGE_CURVE('',#8722,#8721,#1312,.T.);
#10928=EDGE_CURVE('',#8719,#8722,#7499,.T.);
#10929=EDGE_CURVE('',#8723,#8724,#2161,.T.);
#10930=EDGE_CURVE('',#8723,#8725,#7500,.T.);
#10931=EDGE_CURVE('',#8726,#8725,#1313,.T.);
#10932=EDGE_CURVE('',#8724,#8726,#1314,.T.);
#10933=EDGE_CURVE('',#8727,#8728,#2162,.T.);
#10934=EDGE_CURVE('',#8723,#8727,#1315,.T.);
#10935=EDGE_CURVE('',#8728,#8724,#1394,.T.);
#10936=EDGE_CURVE('',#8729,#8728,#1395,.T.);
#10937=EDGE_CURVE('',#8730,#8729,#1316,.T.);
#10938=EDGE_CURVE('',#8727,#8730,#7501,.T.);
#10939=EDGE_CURVE('',#8731,#8732,#1396,.T.);
#10940=EDGE_CURVE('',#8731,#8733,#2163,.T.);
#10941=EDGE_CURVE('',#8734,#8733,#7502,.T.);
#10942=EDGE_CURVE('',#8732,#8734,#1317,.T.);
#10943=EDGE_CURVE('',#8735,#8731,#1397,.T.);
#10944=EDGE_CURVE('',#8735,#8736,#2164,.T.);
#10945=EDGE_CURVE('',#8733,#8736,#1318,.T.);
#10946=EDGE_CURVE('',#8737,#8735,#1319,.T.);
#10947=EDGE_CURVE('',#8738,#8737,#1320,.T.);
#10948=EDGE_CURVE('',#8736,#8738,#7503,.T.);
#10949=EDGE_CURVE('',#8721,#8342,#7504,.T.);
#10950=EDGE_CURVE('',#8739,#8718,#7505,.T.);
#10951=EDGE_CURVE('',#8740,#8739,#7506,.T.);
#10952=EDGE_CURVE('',#8713,#8740,#7507,.T.);
#10953=EDGE_CURVE('',#8741,#8708,#7508,.T.);
#10954=EDGE_CURVE('',#8742,#8741,#7509,.T.);
#10955=EDGE_CURVE('',#8737,#8742,#7510,.T.);
#10956=EDGE_CURVE('',#8743,#8732,#7511,.T.);
#10957=EDGE_CURVE('',#8744,#8743,#7512,.T.);
#10958=EDGE_CURVE('',#8729,#8744,#7513,.T.);
#10959=EDGE_CURVE('',#8343,#8726,#7514,.T.);
#10960=EDGE_CURVE('',#8745,#8746,#2165,.T.);
#10961=EDGE_CURVE('',#8746,#8747,#2166,.T.);
#10962=EDGE_CURVE('',#8747,#8748,#2167,.T.);
#10963=EDGE_CURVE('',#8748,#8749,#2168,.T.);
#10964=EDGE_CURVE('',#8749,#8750,#2169,.T.);
#10965=EDGE_CURVE('',#8750,#8745,#2170,.T.);
#10966=EDGE_CURVE('',#8751,#8752,#2171,.T.);
#10967=EDGE_CURVE('',#8752,#8753,#2172,.T.);
#10968=EDGE_CURVE('',#8753,#8754,#2173,.T.);
#10969=EDGE_CURVE('',#8754,#8755,#2174,.T.);
#10970=EDGE_CURVE('',#8755,#8756,#2175,.T.);
#10971=EDGE_CURVE('',#8756,#8751,#2176,.T.);
#10972=EDGE_CURVE('',#8706,#8695,#2177,.T.);
#10973=EDGE_CURVE('',#8696,#8699,#2178,.T.);
#10974=EDGE_CURVE('',#8700,#8701,#2179,.T.);
#10975=EDGE_CURVE('',#8702,#8705,#2180,.T.);
#10976=EDGE_CURVE('',#8757,#8758,#7515,.T.);
#10977=EDGE_CURVE('',#8741,#8757,#2181,.T.);
#10978=EDGE_CURVE('',#8758,#8708,#1321,.T.);
#10979=EDGE_CURVE('',#8759,#8710,#2182,.T.);
#10980=EDGE_CURVE('',#8758,#8759,#2183,.T.);
#10981=EDGE_CURVE('',#8760,#8714,#2184,.T.);
#10982=EDGE_CURVE('',#8759,#8760,#2185,.T.);
#10983=EDGE_CURVE('',#8761,#8713,#1322,.T.);
#10984=EDGE_CURVE('',#8760,#8761,#2186,.T.);
#10985=EDGE_CURVE('',#8761,#8762,#7516,.T.);
#10986=EDGE_CURVE('',#8762,#8740,#2187,.T.);
#10987=EDGE_CURVE('',#8763,#8739,#2188,.T.);
#10988=EDGE_CURVE('',#8762,#8763,#7517,.T.);
#10989=EDGE_CURVE('',#8763,#8764,#7518,.T.);
#10990=EDGE_CURVE('',#8764,#8718,#1323,.T.);
#10991=EDGE_CURVE('',#8765,#8717,#2189,.T.);
#10992=EDGE_CURVE('',#8764,#8765,#2190,.T.);
#10993=EDGE_CURVE('',#8766,#8722,#2191,.T.);
#10994=EDGE_CURVE('',#8765,#8766,#2192,.T.);
#10995=EDGE_CURVE('',#8767,#8721,#1324,.T.);
#10996=EDGE_CURVE('',#8766,#8767,#2193,.T.);
#10997=EDGE_CURVE('',#8767,#8345,#7519,.T.);
#10998=EDGE_CURVE('',#8344,#8768,#7520,.T.);
#10999=EDGE_CURVE('',#8768,#8726,#1325,.T.);
#11000=EDGE_CURVE('',#8769,#8725,#2194,.T.);
#11001=EDGE_CURVE('',#8768,#8769,#2195,.T.);
#11002=EDGE_CURVE('',#8770,#8730,#2196,.T.);
#11003=EDGE_CURVE('',#8769,#8770,#2197,.T.);
#11004=EDGE_CURVE('',#8771,#8729,#1326,.T.);
#11005=EDGE_CURVE('',#8770,#8771,#2198,.T.);
#11006=EDGE_CURVE('',#8771,#8772,#7521,.T.);
#11007=EDGE_CURVE('',#8772,#8744,#2199,.T.);
#11008=EDGE_CURVE('',#8773,#8743,#2200,.T.);
#11009=EDGE_CURVE('',#8772,#8773,#7522,.T.);
#11010=EDGE_CURVE('',#8773,#8774,#7523,.T.);
#11011=EDGE_CURVE('',#8774,#8732,#1327,.T.);
#11012=EDGE_CURVE('',#8775,#8734,#2201,.T.);
#11013=EDGE_CURVE('',#8774,#8775,#2202,.T.);
#11014=EDGE_CURVE('',#8776,#8738,#2203,.T.);
#11015=EDGE_CURVE('',#8775,#8776,#2204,.T.);
#11016=EDGE_CURVE('',#8777,#8737,#1328,.T.);
#11017=EDGE_CURVE('',#8776,#8777,#2205,.T.);
#11018=EDGE_CURVE('',#8777,#8778,#7524,.T.);
#11019=EDGE_CURVE('',#8778,#8742,#2206,.T.);
#11020=EDGE_CURVE('',#8778,#8757,#7525,.T.);
#11021=EDGE_CURVE('',#8779,#8745,#2207,.T.);
#11022=EDGE_CURVE('',#8750,#8780,#2208,.T.);
#11023=EDGE_CURVE('',#8779,#8780,#2209,.T.);
#11024=EDGE_CURVE('',#8749,#8781,#2210,.T.);
#11025=EDGE_CURVE('',#8780,#8781,#2211,.T.);
#11026=EDGE_CURVE('',#8748,#8782,#2212,.T.);
#11027=EDGE_CURVE('',#8781,#8782,#2213,.T.);
#11028=EDGE_CURVE('',#8747,#8783,#2214,.T.);
#11029=EDGE_CURVE('',#8782,#8783,#2215,.T.);
#11030=EDGE_CURVE('',#8746,#8784,#2216,.T.);
#11031=EDGE_CURVE('',#8783,#8784,#2217,.T.);
#11032=EDGE_CURVE('',#8784,#8779,#2218,.T.);
#11033=EDGE_CURVE('',#8785,#8751,#2219,.T.);
#11034=EDGE_CURVE('',#8756,#8786,#2220,.T.);
#11035=EDGE_CURVE('',#8785,#8786,#2221,.T.);
#11036=EDGE_CURVE('',#8755,#8787,#2222,.T.);
#11037=EDGE_CURVE('',#8786,#8787,#2223,.T.);
#11038=EDGE_CURVE('',#8754,#8788,#2224,.T.);
#11039=EDGE_CURVE('',#8787,#8788,#2225,.T.);
#11040=EDGE_CURVE('',#8753,#8789,#2226,.T.);
#11041=EDGE_CURVE('',#8788,#8789,#2227,.T.);
#11042=EDGE_CURVE('',#8752,#8790,#2228,.T.);
#11043=EDGE_CURVE('',#8789,#8790,#2229,.T.);
#11044=EDGE_CURVE('',#8790,#8785,#2230,.T.);
#11045=EDGE_CURVE('',#8791,#8792,#7526,.T.);
#11046=EDGE_CURVE('',#8793,#8791,#2231,.T.);
#11047=EDGE_CURVE('',#8793,#8794,#7527,.T.);
#11048=EDGE_CURVE('',#8792,#8794,#2232,.T.);
#11049=EDGE_CURVE('',#8795,#8796,#7528,.T.);
#11050=EDGE_CURVE('',#8797,#8796,#2233,.T.);
#11051=EDGE_CURVE('',#8798,#8797,#7529,.T.);
#11052=EDGE_CURVE('',#8795,#8798,#2234,.T.);
#11053=EDGE_CURVE('',#8799,#8800,#2235,.T.);
#11054=EDGE_CURVE('',#8800,#8801,#2236,.T.);
#11055=EDGE_CURVE('',#8801,#8802,#2237,.T.);
#11056=EDGE_CURVE('',#8802,#8799,#2238,.T.);
#11057=EDGE_CURVE('',#8803,#8804,#2239,.T.);
#11058=EDGE_CURVE('',#8805,#8803,#7530,.T.);
#11059=EDGE_CURVE('',#8806,#8805,#2240,.T.);
#11060=EDGE_CURVE('',#8806,#8801,#2241,.T.);
#11061=EDGE_CURVE('',#8800,#8804,#2242,.T.);
#11062=EDGE_CURVE('',#8805,#8807,#2243,.T.);
#11063=EDGE_CURVE('',#8808,#8803,#2244,.T.);
#11064=EDGE_CURVE('',#8807,#8808,#7531,.T.);
#11065=EDGE_CURVE('',#8809,#8810,#7532,.T.);
#11066=EDGE_CURVE('',#8811,#8810,#2245,.T.);
#11067=EDGE_CURVE('',#8812,#8811,#7533,.T.);
#11068=EDGE_CURVE('',#8809,#8812,#2246,.T.);
#11069=EDGE_CURVE('',#8813,#8814,#7534,.T.);
#11070=EDGE_CURVE('',#8815,#8813,#2247,.T.);
#11071=EDGE_CURVE('',#8815,#8816,#7535,.T.);
#11072=EDGE_CURVE('',#8814,#8816,#2248,.T.);
#11073=EDGE_CURVE('',#8817,#8818,#7536,.T.);
#11074=EDGE_CURVE('',#8819,#8818,#2249,.T.);
#11075=EDGE_CURVE('',#8820,#8819,#7537,.T.);
#11076=EDGE_CURVE('',#8817,#8820,#2250,.T.);
#11077=EDGE_CURVE('',#8813,#8819,#2251,.T.);
#11078=EDGE_CURVE('',#8812,#8814,#2252,.T.);
#11079=EDGE_CURVE('',#8807,#8811,#2253,.T.);
#11080=EDGE_CURVE('',#8798,#8808,#2254,.T.);
#11081=EDGE_CURVE('',#8791,#8797,#2255,.T.);
#11082=EDGE_CURVE('',#8821,#8792,#2256,.T.);
#11083=EDGE_CURVE('',#8822,#8821,#7538,.T.);
#11084=EDGE_CURVE('',#8339,#8822,#2257,.T.);
#11085=EDGE_CURVE('',#8820,#8338,#2258,.T.);
#11086=EDGE_CURVE('',#8823,#8824,#7539,.T.);
#11087=EDGE_CURVE('',#8822,#8824,#2259,.T.);
#11088=EDGE_CURVE('',#8823,#8821,#2260,.T.);
#11089=EDGE_CURVE('',#8794,#8825,#2261,.T.);
#11090=EDGE_CURVE('',#8825,#8826,#2262,.T.);
#11091=EDGE_CURVE('',#8826,#8823,#2263,.T.);
#11092=EDGE_CURVE('',#8796,#8827,#2264,.T.);
#11093=EDGE_CURVE('',#8827,#8828,#2265,.T.);
#11094=EDGE_CURVE('',#8828,#8793,#2266,.T.);
#11095=EDGE_CURVE('',#8828,#8829,#2267,.T.);
#11096=EDGE_CURVE('',#8830,#8829,#7540,.T.);
#11097=EDGE_CURVE('',#8830,#8831,#2268,.T.);
#11098=EDGE_CURVE('',#8831,#8832,#2269,.T.);
#11099=EDGE_CURVE('',#8832,#8833,#2270,.T.);
#11100=EDGE_CURVE('',#8834,#8833,#7541,.T.);
#11101=EDGE_CURVE('',#8834,#8825,#2271,.T.);
#11102=EDGE_CURVE('',#8835,#8836,#2272,.T.);
#11103=EDGE_CURVE('',#8837,#8836,#7542,.T.);
#11104=EDGE_CURVE('',#8837,#8838,#2273,.T.);
#11105=EDGE_CURVE('',#8838,#8835,#7543,.T.);
#11106=EDGE_CURVE('',#8804,#8839,#2274,.T.);
#11107=EDGE_CURVE('',#8839,#8840,#2275,.T.);
#11108=EDGE_CURVE('',#8840,#8841,#2276,.T.);
#11109=EDGE_CURVE('',#8841,#8795,#2277,.T.);
#11110=EDGE_CURVE('',#8841,#8835,#2278,.T.);
#11111=EDGE_CURVE('',#8838,#8827,#2279,.T.);
#11112=EDGE_CURVE('',#8842,#8843,#2280,.T.);
#11113=EDGE_CURVE('',#8844,#8842,#7544,.T.);
#11114=EDGE_CURVE('',#8844,#8840,#2281,.T.);
#11115=EDGE_CURVE('',#8839,#8843,#2282,.T.);
#11116=EDGE_CURVE('',#8845,#8843,#2283,.T.);
#11117=EDGE_CURVE('',#8799,#8845,#2284,.T.);
#11118=EDGE_CURVE('',#8846,#8847,#2285,.T.);
#11119=EDGE_CURVE('',#8847,#8802,#2286,.T.);
#11120=EDGE_CURVE('',#8848,#8806,#2287,.T.);
#11121=EDGE_CURVE('',#8848,#8846,#2288,.T.);
#11122=EDGE_CURVE('',#8847,#8849,#2289,.T.);
#11123=EDGE_CURVE('',#8849,#8850,#2290,.T.);
#11124=EDGE_CURVE('',#8850,#8845,#2291,.T.);
#11125=EDGE_CURVE('',#8851,#8852,#2292,.T.);
#11126=EDGE_CURVE('',#8852,#8848,#2293,.T.);
#11127=EDGE_CURVE('',#8810,#8851,#2294,.T.);
#11128=EDGE_CURVE('',#8852,#8853,#2295,.T.);
#11129=EDGE_CURVE('',#8854,#8853,#7545,.T.);
#11130=EDGE_CURVE('',#8854,#8846,#2296,.T.);
#11131=EDGE_CURVE('',#8855,#8856,#2297,.T.);
#11132=EDGE_CURVE('',#8857,#8856,#7546,.T.);
#11133=EDGE_CURVE('',#8857,#8858,#2298,.T.);
#11134=EDGE_CURVE('',#8858,#8855,#7547,.T.);
#11135=EDGE_CURVE('',#8816,#8859,#2299,.T.);
#11136=EDGE_CURVE('',#8859,#8860,#2300,.T.);
#11137=EDGE_CURVE('',#8860,#8809,#2301,.T.);
#11138=EDGE_CURVE('',#8860,#8855,#2302,.T.);
#11139=EDGE_CURVE('',#8858,#8851,#2303,.T.);
#11140=EDGE_CURVE('',#8818,#8861,#2304,.T.);
#11141=EDGE_CURVE('',#8861,#8862,#2305,.T.);
#11142=EDGE_CURVE('',#8862,#8815,#2306,.T.);
#11143=EDGE_CURVE('',#8862,#8863,#2307,.T.);
#11144=EDGE_CURVE('',#8864,#8863,#7548,.T.);
#11145=EDGE_CURVE('',#8864,#8865,#2308,.T.);
#11146=EDGE_CURVE('',#8865,#8866,#2309,.T.);
#11147=EDGE_CURVE('',#8866,#8867,#2310,.T.);
#11148=EDGE_CURVE('',#8868,#8867,#7549,.T.);
#11149=EDGE_CURVE('',#8868,#8859,#2311,.T.);
#11150=EDGE_CURVE('',#8869,#8870,#2312,.T.);
#11151=EDGE_CURVE('',#8871,#8870,#7550,.T.);
#11152=EDGE_CURVE('',#8871,#8872,#2313,.T.);
#11153=EDGE_CURVE('',#8872,#8869,#7551,.T.);
#11154=EDGE_CURVE('',#8337,#8873,#2314,.T.);
#11155=EDGE_CURVE('',#8873,#8874,#2315,.T.);
#11156=EDGE_CURVE('',#8874,#8817,#2316,.T.);
#11157=EDGE_CURVE('',#8874,#8869,#2317,.T.);
#11158=EDGE_CURVE('',#8872,#8861,#2318,.T.);
#11159=EDGE_CURVE('',#8875,#8876,#2319,.T.);
#11160=EDGE_CURVE('',#8877,#8876,#7552,.T.);
#11161=EDGE_CURVE('',#8877,#8878,#2320,.T.);
#11162=EDGE_CURVE('',#8878,#8875,#7553,.T.);
#11163=EDGE_CURVE('',#8826,#8875,#2321,.T.);
#11164=EDGE_CURVE('',#8878,#8879,#2322,.T.);
#11165=EDGE_CURVE('',#8824,#8879,#2323,.T.);
#11166=EDGE_CURVE('',#8879,#8880,#2324,.T.);
#11167=EDGE_CURVE('',#8880,#8336,#2325,.T.);
#11168=EDGE_CURVE('',#8880,#8881,#2326,.T.);
#11169=EDGE_CURVE('',#8882,#8881,#7554,.T.);
#11170=EDGE_CURVE('',#8882,#8883,#2327,.T.);
#11171=EDGE_CURVE('',#8883,#8884,#2328,.T.);
#11172=EDGE_CURVE('',#8884,#8885,#2329,.T.);
#11173=EDGE_CURVE('',#8886,#8885,#7555,.T.);
#11174=EDGE_CURVE('',#8886,#8873,#2330,.T.);
#11175=EDGE_CURVE('',#8887,#8888,#2331,.T.);
#11176=EDGE_CURVE('',#8888,#8889,#2332,.T.);
#11177=EDGE_CURVE('',#8889,#8890,#2333,.T.);
#11178=EDGE_CURVE('',#8890,#8891,#2334,.T.);
#11179=EDGE_CURVE('',#8891,#8892,#2335,.T.);
#11180=EDGE_CURVE('',#8892,#8887,#2336,.T.);
#11181=EDGE_CURVE('',#8893,#8894,#2337,.T.);
#11182=EDGE_CURVE('',#8894,#8895,#2338,.T.);
#11183=EDGE_CURVE('',#8896,#8895,#2339,.T.);
#11184=EDGE_CURVE('',#8896,#8893,#2340,.T.);
#11185=EDGE_CURVE('',#8897,#8898,#2341,.T.);
#11186=EDGE_CURVE('',#8898,#8877,#2342,.T.);
#11187=EDGE_CURVE('',#8876,#8899,#2343,.T.);
#11188=EDGE_CURVE('',#8899,#8900,#2344,.T.);
#11189=EDGE_CURVE('',#8897,#8900,#7556,.T.);
#11190=EDGE_CURVE('',#8900,#8901,#2345,.T.);
#11191=EDGE_CURVE('',#8901,#8902,#7557,.T.);
#11192=EDGE_CURVE('',#8902,#8897,#2346,.T.);
#11193=EDGE_CURVE('',#8903,#8834,#2347,.T.);
#11194=EDGE_CURVE('',#8904,#8903,#2348,.T.);
#11195=EDGE_CURVE('',#8904,#8899,#2349,.T.);
#11196=EDGE_CURVE('',#8833,#8905,#2350,.T.);
#11197=EDGE_CURVE('',#8903,#8905,#7558,.T.);
#11198=EDGE_CURVE('',#8832,#8906,#2351,.T.);
#11199=EDGE_CURVE('',#8905,#8906,#2352,.T.);
#11200=EDGE_CURVE('',#8831,#8907,#2353,.T.);
#11201=EDGE_CURVE('',#8906,#8907,#2354,.T.);
#11202=EDGE_CURVE('',#8908,#8830,#2355,.T.);
#11203=EDGE_CURVE('',#8907,#8908,#2356,.T.);
#11204=EDGE_CURVE('',#8829,#8909,#2357,.T.);
#11205=EDGE_CURVE('',#8908,#8909,#7559,.T.);
#11206=EDGE_CURVE('',#8910,#8837,#2358,.T.);
#11207=EDGE_CURVE('',#8910,#8911,#2359,.T.);
#11208=EDGE_CURVE('',#8909,#8911,#2360,.T.);
#11209=EDGE_CURVE('',#8912,#8910,#2361,.T.);
#11210=EDGE_CURVE('',#8836,#8913,#2362,.T.);
#11211=EDGE_CURVE('',#8913,#8914,#2363,.T.);
#11212=EDGE_CURVE('',#8912,#8914,#7560,.T.);
#11213=EDGE_CURVE('',#8914,#8915,#2364,.T.);
#11214=EDGE_CURVE('',#8915,#8916,#7561,.T.);
#11215=EDGE_CURVE('',#8916,#8912,#2365,.T.);
#11216=EDGE_CURVE('',#8917,#8844,#2366,.T.);
#11217=EDGE_CURVE('',#8918,#8917,#2367,.T.);
#11218=EDGE_CURVE('',#8918,#8913,#2368,.T.);
#11219=EDGE_CURVE('',#8842,#8919,#2369,.T.);
#11220=EDGE_CURVE('',#8917,#8919,#7562,.T.);
#11221=EDGE_CURVE('',#8850,#8920,#2370,.T.);
#11222=EDGE_CURVE('',#8919,#8920,#2371,.T.);
#11223=EDGE_CURVE('',#8849,#8921,#2372,.T.);
#11224=EDGE_CURVE('',#8920,#8921,#2373,.T.);
#11225=EDGE_CURVE('',#8922,#8854,#2374,.T.);
#11226=EDGE_CURVE('',#8921,#8922,#2375,.T.);
#11227=EDGE_CURVE('',#8853,#8923,#2376,.T.);
#11228=EDGE_CURVE('',#8922,#8923,#7563,.T.);
#11229=EDGE_CURVE('',#8924,#8857,#2377,.T.);
#11230=EDGE_CURVE('',#8924,#8925,#2378,.T.);
#11231=EDGE_CURVE('',#8923,#8925,#2379,.T.);
#11232=EDGE_CURVE('',#8926,#8924,#2380,.T.);
#11233=EDGE_CURVE('',#8856,#8927,#2381,.T.);
#11234=EDGE_CURVE('',#8927,#8928,#2382,.T.);
#11235=EDGE_CURVE('',#8926,#8928,#7564,.T.);
#11236=EDGE_CURVE('',#8928,#8929,#2383,.T.);
#11237=EDGE_CURVE('',#8929,#8930,#7565,.T.);
#11238=EDGE_CURVE('',#8930,#8926,#2384,.T.);
#11239=EDGE_CURVE('',#8931,#8868,#2385,.T.);
#11240=EDGE_CURVE('',#8932,#8931,#2386,.T.);
#11241=EDGE_CURVE('',#8932,#8927,#2387,.T.);
#11242=EDGE_CURVE('',#8867,#8933,#2388,.T.);
#11243=EDGE_CURVE('',#8931,#8933,#7566,.T.);
#11244=EDGE_CURVE('',#8866,#8934,#2389,.T.);
#11245=EDGE_CURVE('',#8933,#8934,#2390,.T.);
#11246=EDGE_CURVE('',#8865,#8935,#2391,.T.);
#11247=EDGE_CURVE('',#8934,#8935,#2392,.T.);
#11248=EDGE_CURVE('',#8936,#8864,#2393,.T.);
#11249=EDGE_CURVE('',#8935,#8936,#2394,.T.);
#11250=EDGE_CURVE('',#8863,#8937,#2395,.T.);
#11251=EDGE_CURVE('',#8936,#8937,#7567,.T.);
#11252=EDGE_CURVE('',#8938,#8871,#2396,.T.);
#11253=EDGE_CURVE('',#8938,#8939,#2397,.T.);
#11254=EDGE_CURVE('',#8937,#8939,#2398,.T.);
#11255=EDGE_CURVE('',#8940,#8938,#2399,.T.);
#11256=EDGE_CURVE('',#8870,#8941,#2400,.T.);
#11257=EDGE_CURVE('',#8941,#8942,#2401,.T.);
#11258=EDGE_CURVE('',#8940,#8942,#7568,.T.);
#11259=EDGE_CURVE('',#8942,#8943,#2402,.T.);
#11260=EDGE_CURVE('',#8943,#8944,#7569,.T.);
#11261=EDGE_CURVE('',#8944,#8940,#2403,.T.);
#11262=EDGE_CURVE('',#8945,#8886,#2404,.T.);
#11263=EDGE_CURVE('',#8946,#8945,#2405,.T.);
#11264=EDGE_CURVE('',#8946,#8941,#2406,.T.);
#11265=EDGE_CURVE('',#8885,#8947,#2407,.T.);
#11266=EDGE_CURVE('',#8945,#8947,#7570,.T.);
#11267=EDGE_CURVE('',#8884,#8948,#2408,.T.);
#11268=EDGE_CURVE('',#8947,#8948,#2409,.T.);
#11269=EDGE_CURVE('',#8883,#8949,#2410,.T.);
#11270=EDGE_CURVE('',#8948,#8949,#2411,.T.);
#11271=EDGE_CURVE('',#8950,#8882,#2412,.T.);
#11272=EDGE_CURVE('',#8949,#8950,#2413,.T.);
#11273=EDGE_CURVE('',#8881,#8951,#2414,.T.);
#11274=EDGE_CURVE('',#8950,#8951,#7571,.T.);
#11275=EDGE_CURVE('',#8898,#8952,#2415,.T.);
#11276=EDGE_CURVE('',#8951,#8952,#2416,.T.);
#11277=EDGE_CURVE('',#8892,#8953,#2417,.T.);
#11278=EDGE_CURVE('',#8954,#8953,#2418,.T.);
#11279=EDGE_CURVE('',#8954,#8887,#2419,.T.);
#11280=EDGE_CURVE('',#8891,#8955,#2420,.T.);
#11281=EDGE_CURVE('',#8953,#8955,#2421,.T.);
#11282=EDGE_CURVE('',#8890,#8956,#2422,.T.);
#11283=EDGE_CURVE('',#8955,#8956,#2423,.T.);
#11284=EDGE_CURVE('',#8889,#8957,#2424,.T.);
#11285=EDGE_CURVE('',#8956,#8957,#2425,.T.);
#11286=EDGE_CURVE('',#8888,#8958,#2426,.T.);
#11287=EDGE_CURVE('',#8957,#8958,#2427,.T.);
#11288=EDGE_CURVE('',#8958,#8954,#2428,.T.);
#11289=EDGE_CURVE('',#8895,#8317,#2429,.T.);
#11290=EDGE_CURVE('',#8894,#8318,#2430,.T.);
#11291=EDGE_CURVE('',#8893,#8313,#2431,.T.);
#11292=EDGE_CURVE('',#8314,#8896,#2432,.T.);
#11293=EDGE_CURVE('',#8902,#8959,#2433,.T.);
#11294=EDGE_CURVE('',#8960,#8959,#2434,.T.);
#11295=EDGE_CURVE('',#8952,#8960,#2435,.T.);
#11296=EDGE_CURVE('',#8961,#8962,#2436,.T.);
#11297=EDGE_CURVE('',#8963,#8961,#7572,.T.);
#11298=EDGE_CURVE('',#8964,#8963,#2437,.T.);
#11299=EDGE_CURVE('',#8959,#8964,#7573,.T.);
#11300=EDGE_CURVE('',#8901,#8965,#2438,.T.);
#11301=EDGE_CURVE('',#8962,#8965,#7574,.T.);
#11302=EDGE_CURVE('',#8966,#8904,#2439,.T.);
#11303=EDGE_CURVE('',#8965,#8966,#2440,.T.);
#11304=EDGE_CURVE('',#8911,#8967,#2441,.T.);
#11305=EDGE_CURVE('',#8966,#8967,#7575,.T.);
#11306=EDGE_CURVE('',#8916,#8968,#2442,.T.);
#11307=EDGE_CURVE('',#8967,#8968,#2443,.T.);
#11308=EDGE_CURVE('',#8969,#8300,#2444,.T.);
#11309=EDGE_CURVE('',#8970,#8969,#7576,.T.);
#11310=EDGE_CURVE('',#8971,#8970,#2445,.T.);
#11311=EDGE_CURVE('',#8968,#8971,#7577,.T.);
#11312=EDGE_CURVE('',#8915,#8301,#2446,.T.);
#11313=EDGE_CURVE('',#8296,#8918,#2447,.T.);
#11314=EDGE_CURVE('',#8925,#8297,#2448,.T.);
#11315=EDGE_CURVE('',#8930,#8298,#2449,.T.);
#11316=EDGE_CURVE('',#8929,#8972,#2450,.T.);
#11317=EDGE_CURVE('',#8973,#8972,#7578,.T.);
#11318=EDGE_CURVE('',#8974,#8973,#2451,.T.);
#11319=EDGE_CURVE('',#8975,#8974,#7579,.T.);
#11320=EDGE_CURVE('',#8299,#8975,#2452,.T.);
#11321=EDGE_CURVE('',#8976,#8932,#2453,.T.);
#11322=EDGE_CURVE('',#8972,#8976,#2454,.T.);
#11323=EDGE_CURVE('',#8939,#8977,#2455,.T.);
#11324=EDGE_CURVE('',#8976,#8977,#7580,.T.);
#11325=EDGE_CURVE('',#8944,#8978,#2456,.T.);
#11326=EDGE_CURVE('',#8977,#8978,#2457,.T.);
#11327=EDGE_CURVE('',#8943,#8979,#2458,.T.);
#11328=EDGE_CURVE('',#8980,#8979,#7581,.T.);
#11329=EDGE_CURVE('',#8981,#8980,#2459,.T.);
#11330=EDGE_CURVE('',#8982,#8981,#7582,.T.);
#11331=EDGE_CURVE('',#8983,#8982,#2460,.T.);
#11332=EDGE_CURVE('',#8978,#8983,#7583,.T.);
#11333=EDGE_CURVE('',#8984,#8946,#2461,.T.);
#11334=EDGE_CURVE('',#8979,#8984,#2462,.T.);
#11335=EDGE_CURVE('',#8984,#8960,#7584,.T.);
#11336=EDGE_CURVE('',#8985,#8986,#2463,.T.);
#11337=EDGE_CURVE('',#8986,#8987,#2464,.T.);
#11338=EDGE_CURVE('',#8987,#8988,#2465,.T.);
#11339=EDGE_CURVE('',#8988,#8989,#2466,.T.);
#11340=EDGE_CURVE('',#8989,#8990,#2467,.T.);
#11341=EDGE_CURVE('',#8990,#8985,#2468,.T.);
#11342=EDGE_CURVE('',#8273,#8963,#2469,.T.);
#11343=EDGE_CURVE('',#8272,#8964,#2470,.T.);
#11344=EDGE_CURVE('',#8274,#8961,#2471,.T.);
#11345=EDGE_CURVE('',#8275,#8962,#2472,.T.);
#11346=EDGE_CURVE('',#8279,#8971,#2473,.T.);
#11347=EDGE_CURVE('',#8280,#8970,#2474,.T.);
#11348=EDGE_CURVE('',#8281,#8969,#2475,.T.);
#11349=EDGE_CURVE('',#8284,#8975,#2476,.T.);
#11350=EDGE_CURVE('',#8285,#8974,#2477,.T.);
#11351=EDGE_CURVE('',#8267,#8973,#2478,.T.);
#11352=EDGE_CURVE('',#8268,#8983,#2479,.T.);
#11353=EDGE_CURVE('',#8269,#8982,#2480,.T.);
#11354=EDGE_CURVE('',#8270,#8981,#2481,.T.);
#11355=EDGE_CURVE('',#8271,#8980,#2482,.T.);
#11356=EDGE_CURVE('',#8991,#8992,#2483,.T.);
#11357=EDGE_CURVE('',#8993,#8991,#2484,.T.);
#11358=EDGE_CURVE('',#8994,#8993,#2485,.T.);
#11359=EDGE_CURVE('',#8995,#8994,#2486,.T.);
#11360=EDGE_CURVE('',#8996,#8995,#2487,.T.);
#11361=EDGE_CURVE('',#8997,#8996,#2488,.T.);
#11362=EDGE_CURVE('',#8998,#8997,#2489,.T.);
#11363=EDGE_CURVE('',#8992,#8998,#2490,.T.);
#11364=EDGE_CURVE('',#8292,#8995,#7585,.T.);
#11365=EDGE_CURVE('',#8996,#8293,#7586,.T.);
#11366=EDGE_CURVE('',#8999,#8294,#7587,.T.);
#11367=EDGE_CURVE('',#9000,#8999,#2491,.T.);
#11368=EDGE_CURVE('',#8295,#9000,#7588,.T.);
#11369=EDGE_CURVE('',#9001,#9002,#2492,.T.);
#11370=EDGE_CURVE('',#9003,#9001,#2493,.T.);
#11371=EDGE_CURVE('',#9004,#9003,#2494,.T.);
#11372=EDGE_CURVE('',#9004,#9005,#2495,.T.);
#11373=EDGE_CURVE('',#9006,#9005,#2496,.T.);
#11374=EDGE_CURVE('',#9000,#9006,#2497,.T.);
#11375=EDGE_CURVE('',#9002,#8999,#2498,.T.);
#11376=EDGE_CURVE('',#9007,#9008,#2499,.T.);
#11377=EDGE_CURVE('',#9008,#9009,#2500,.T.);
#11378=EDGE_CURVE('',#9009,#9010,#2501,.T.);
#11379=EDGE_CURVE('',#9010,#9011,#2502,.T.);
#11380=EDGE_CURVE('',#9011,#9012,#2503,.T.);
#11381=EDGE_CURVE('',#9012,#9007,#2504,.T.);
#11382=EDGE_CURVE('',#8266,#8227,#1329,.T.);
#11383=EDGE_CURVE('',#8989,#9013,#2505,.T.);
#11384=EDGE_CURVE('',#9013,#9014,#2506,.T.);
#11385=EDGE_CURVE('',#9014,#8990,#2507,.T.);
#11386=EDGE_CURVE('',#9014,#9015,#2508,.T.);
#11387=EDGE_CURVE('',#9015,#8985,#2509,.T.);
#11388=EDGE_CURVE('',#9015,#9016,#2510,.T.);
#11389=EDGE_CURVE('',#9016,#8986,#2511,.T.);
#11390=EDGE_CURVE('',#9016,#9017,#2512,.T.);
#11391=EDGE_CURVE('',#9017,#8987,#2513,.T.);
#11392=EDGE_CURVE('',#9017,#9018,#2514,.T.);
#11393=EDGE_CURVE('',#9018,#8988,#2515,.T.);
#11394=EDGE_CURVE('',#9018,#9013,#2516,.T.);
#11395=EDGE_CURVE('',#9019,#8265,#2517,.T.);
#11396=EDGE_CURVE('',#9019,#9020,#7589,.T.);
#11397=EDGE_CURVE('',#8228,#9020,#2518,.T.);
#11398=EDGE_CURVE('',#8255,#9003,#7590,.T.);
#11399=EDGE_CURVE('',#9004,#8256,#7591,.T.);
#11400=EDGE_CURVE('',#9021,#9022,#1398,.T.);
#11401=EDGE_CURVE('',#9021,#9022,#7592,.T.);
#11402=EDGE_CURVE('',#8289,#9021,#2519,.T.);
#11403=EDGE_CURVE('',#9022,#8288,#2520,.T.);
#11404=EDGE_CURVE('',#9023,#9024,#2521,.T.);
#11405=EDGE_CURVE('',#9024,#9025,#2522,.T.);
#11406=EDGE_CURVE('',#9025,#9026,#2523,.T.);
#11407=EDGE_CURVE('',#9026,#9027,#2524,.T.);
#11408=EDGE_CURVE('',#9027,#9028,#2525,.T.);
#11409=EDGE_CURVE('',#9028,#9023,#2526,.T.);
#11410=EDGE_CURVE('',#9029,#9030,#2527,.T.);
#11411=EDGE_CURVE('',#9030,#9031,#2528,.T.);
#11412=EDGE_CURVE('',#9031,#9032,#2529,.T.);
#11413=EDGE_CURVE('',#9032,#9033,#2530,.T.);
#11414=EDGE_CURVE('',#9033,#9034,#2531,.T.);
#11415=EDGE_CURVE('',#9034,#9029,#2532,.T.);
#11416=EDGE_CURVE('',#9035,#9036,#2533,.T.);
#11417=EDGE_CURVE('',#9036,#9037,#2534,.T.);
#11418=EDGE_CURVE('',#9037,#9038,#2535,.T.);
#11419=EDGE_CURVE('',#9038,#9039,#2536,.T.);
#11420=EDGE_CURVE('',#9039,#9040,#2537,.T.);
#11421=EDGE_CURVE('',#9040,#9035,#2538,.T.);
#11422=EDGE_CURVE('',#9003,#9041,#7593,.T.);
#11423=EDGE_CURVE('',#9041,#9001,#2539,.T.);
#11424=EDGE_CURVE('',#9042,#9002,#2540,.T.);
#11425=EDGE_CURVE('',#9041,#9042,#2541,.T.);
#11426=EDGE_CURVE('',#9042,#8999,#7594,.T.);
#11427=EDGE_CURVE('',#8995,#9043,#7595,.T.);
#11428=EDGE_CURVE('',#9043,#8994,#2542,.T.);
#11429=EDGE_CURVE('',#9044,#8993,#2543,.T.);
#11430=EDGE_CURVE('',#9043,#9044,#2544,.T.);
#11431=EDGE_CURVE('',#9044,#8991,#7596,.T.);
#11432=EDGE_CURVE('',#8991,#8234,#7597,.T.);
#11433=EDGE_CURVE('',#8235,#8992,#7598,.T.);
#11434=EDGE_CURVE('',#8992,#9045,#7599,.T.);
#11435=EDGE_CURVE('',#9045,#8998,#2545,.T.);
#11436=EDGE_CURVE('',#9046,#8997,#2546,.T.);
#11437=EDGE_CURVE('',#9045,#9046,#2547,.T.);
#11438=EDGE_CURVE('',#9046,#8996,#7600,.T.);
#11439=EDGE_CURVE('',#9000,#9047,#7601,.T.);
#11440=EDGE_CURVE('',#9047,#9006,#2548,.T.);
#11441=EDGE_CURVE('',#9048,#9005,#2549,.T.);
#11442=EDGE_CURVE('',#9047,#9048,#2550,.T.);
#11443=EDGE_CURVE('',#9048,#9004,#7602,.T.);
#11444=EDGE_CURVE('',#9011,#9049,#2551,.T.);
#11445=EDGE_CURVE('',#9050,#9049,#2552,.T.);
#11446=EDGE_CURVE('',#9050,#9012,#2553,.T.);
#11447=EDGE_CURVE('',#9010,#9051,#2554,.T.);
#11448=EDGE_CURVE('',#9049,#9051,#2555,.T.);
#11449=EDGE_CURVE('',#9009,#9052,#2556,.T.);
#11450=EDGE_CURVE('',#9051,#9052,#2557,.T.);
#11451=EDGE_CURVE('',#9008,#9053,#2558,.T.);
#11452=EDGE_CURVE('',#9052,#9053,#2559,.T.);
#11453=EDGE_CURVE('',#9007,#9054,#2560,.T.);
#11454=EDGE_CURVE('',#9053,#9054,#2561,.T.);
#11455=EDGE_CURVE('',#9054,#9050,#2562,.T.);
#11456=EDGE_CURVE('',#8229,#9055,#1399,.T.);
#11457=EDGE_CURVE('',#9020,#9056,#2563,.T.);
#11458=EDGE_CURVE('',#9055,#9056,#2564,.T.);
#11459=EDGE_CURVE('',#9056,#9057,#7603,.T.);
#11460=EDGE_CURVE('',#9055,#9057,#1330,.T.);
#11461=EDGE_CURVE('',#9058,#9019,#2565,.T.);
#11462=EDGE_CURVE('',#9059,#9058,#7604,.T.);
#11463=EDGE_CURVE('',#9057,#9059,#2566,.T.);
#11464=EDGE_CURVE('',#9060,#9058,#2567,.T.);
#11465=EDGE_CURVE('',#9059,#9060,#1331,.T.);
#11466=EDGE_CURVE('',#9061,#8264,#1400,.T.);
#11467=EDGE_CURVE('',#9060,#9061,#1401,.T.);
#11468=EDGE_CURVE('',#9062,#9063,#2568,.T.);
#11469=EDGE_CURVE('',#9063,#9064,#2569,.T.);
#11470=EDGE_CURVE('',#9064,#9065,#2570,.T.);
#11471=EDGE_CURVE('',#9065,#9066,#2571,.T.);
#11472=EDGE_CURVE('',#9066,#9067,#2572,.T.);
#11473=EDGE_CURVE('',#9067,#9062,#2573,.T.);
#11474=EDGE_CURVE('',#9068,#9069,#2574,.T.);
#11475=EDGE_CURVE('',#9069,#9070,#2575,.T.);
#11476=EDGE_CURVE('',#9070,#9071,#2576,.T.);
#11477=EDGE_CURVE('',#9071,#9072,#2577,.T.);
#11478=EDGE_CURVE('',#9072,#9073,#2578,.T.);
#11479=EDGE_CURVE('',#9073,#9068,#2579,.T.);
#11480=EDGE_CURVE('',#9074,#9075,#2580,.T.);
#11481=EDGE_CURVE('',#9075,#9076,#2581,.T.);
#11482=EDGE_CURVE('',#9076,#9077,#2582,.T.);
#11483=EDGE_CURVE('',#9077,#9078,#2583,.T.);
#11484=EDGE_CURVE('',#9078,#9079,#2584,.T.);
#11485=EDGE_CURVE('',#9079,#9074,#2585,.T.);
#11486=EDGE_CURVE('',#8244,#9080,#2586,.T.);
#11487=EDGE_CURVE('',#9080,#8277,#2587,.T.);
#11488=EDGE_CURVE('',#9080,#9081,#2588,.T.);
#11489=EDGE_CURVE('',#9081,#8278,#2589,.T.);
#11490=EDGE_CURVE('',#9081,#8243,#2590,.T.);
#11491=EDGE_CURVE('',#9082,#9083,#2591,.T.);
#11492=EDGE_CURVE('',#9083,#9084,#2592,.T.);
#11493=EDGE_CURVE('',#9084,#9085,#2593,.T.);
#11494=EDGE_CURVE('',#9085,#9086,#2594,.T.);
#11495=EDGE_CURVE('',#9086,#9087,#2595,.T.);
#11496=EDGE_CURVE('',#9087,#9082,#2596,.T.);
#11497=EDGE_CURVE('',#9088,#9089,#2597,.T.);
#11498=EDGE_CURVE('',#9089,#9090,#2598,.T.);
#11499=EDGE_CURVE('',#9090,#9091,#2599,.T.);
#11500=EDGE_CURVE('',#9091,#9092,#2600,.T.);
#11501=EDGE_CURVE('',#9092,#9093,#2601,.T.);
#11502=EDGE_CURVE('',#9093,#9088,#2602,.T.);
#11503=EDGE_CURVE('',#9094,#9023,#2603,.T.);
#11504=EDGE_CURVE('',#9028,#9095,#2604,.T.);
#11505=EDGE_CURVE('',#9094,#9095,#2605,.T.);
#11506=EDGE_CURVE('',#9027,#9096,#2606,.T.);
#11507=EDGE_CURVE('',#9095,#9096,#2607,.T.);
#11508=EDGE_CURVE('',#9026,#9097,#2608,.T.);
#11509=EDGE_CURVE('',#9096,#9097,#2609,.T.);
#11510=EDGE_CURVE('',#9025,#9098,#2610,.T.);
#11511=EDGE_CURVE('',#9097,#9098,#2611,.T.);
#11512=EDGE_CURVE('',#9024,#9099,#2612,.T.);
#11513=EDGE_CURVE('',#9098,#9099,#2613,.T.);
#11514=EDGE_CURVE('',#9099,#9094,#2614,.T.);
#11515=EDGE_CURVE('',#9100,#9101,#2615,.T.);
#11516=EDGE_CURVE('',#9102,#9101,#7605,.T.);
#11517=EDGE_CURVE('',#9102,#9100,#2616,.T.);
#11518=EDGE_CURVE('',#9103,#9104,#2617,.T.);
#11519=EDGE_CURVE('',#9103,#9101,#7606,.T.);
#11520=EDGE_CURVE('',#9100,#9104,#7607,.T.);
#11521=EDGE_CURVE('',#9104,#9105,#2618,.T.);
#11522=EDGE_CURVE('',#9105,#9106,#2619,.T.);
#11523=EDGE_CURVE('',#9107,#9106,#7608,.T.);
#11524=EDGE_CURVE('',#9107,#9103,#2620,.T.);
#11525=EDGE_CURVE('',#9033,#9108,#2621,.T.);
#11526=EDGE_CURVE('',#9108,#9109,#2622,.T.);
#11527=EDGE_CURVE('',#9109,#9034,#2623,.T.);
#11528=EDGE_CURVE('',#9109,#9110,#2624,.T.);
#11529=EDGE_CURVE('',#9110,#9029,#2625,.T.);
#11530=EDGE_CURVE('',#9110,#9111,#2626,.T.);
#11531=EDGE_CURVE('',#9111,#9030,#2627,.T.);
#11532=EDGE_CURVE('',#9111,#9112,#2628,.T.);
#11533=EDGE_CURVE('',#9112,#9031,#2629,.T.);
#11534=EDGE_CURVE('',#9112,#9113,#2630,.T.);
#11535=EDGE_CURVE('',#9113,#9032,#2631,.T.);
#11536=EDGE_CURVE('',#9113,#9108,#2632,.T.);
#11537=EDGE_CURVE('',#9114,#9115,#2633,.T.);
#11538=EDGE_CURVE('',#9114,#9116,#7609,.T.);
#11539=EDGE_CURVE('',#9117,#9116,#2634,.T.);
#11540=EDGE_CURVE('',#9115,#9117,#7610,.T.);
#11541=EDGE_CURVE('',#9116,#9118,#2635,.T.);
#11542=EDGE_CURVE('',#9119,#9118,#7611,.T.);
#11543=EDGE_CURVE('',#9119,#9120,#2636,.T.);
#11544=EDGE_CURVE('',#9117,#9120,#2637,.T.);
#11545=EDGE_CURVE('',#9039,#9121,#2638,.T.);
#11546=EDGE_CURVE('',#9122,#9121,#2639,.T.);
#11547=EDGE_CURVE('',#9122,#9040,#2640,.T.);
#11548=EDGE_CURVE('',#9038,#9123,#2641,.T.);
#11549=EDGE_CURVE('',#9121,#9123,#2642,.T.);
#11550=EDGE_CURVE('',#9037,#9124,#2643,.T.);
#11551=EDGE_CURVE('',#9123,#9124,#2644,.T.);
#11552=EDGE_CURVE('',#9036,#9125,#2645,.T.);
#11553=EDGE_CURVE('',#9124,#9125,#2646,.T.);
#11554=EDGE_CURVE('',#9035,#9126,#2647,.T.);
#11555=EDGE_CURVE('',#9125,#9126,#2648,.T.);
#11556=EDGE_CURVE('',#9126,#9122,#2649,.T.);
#11557=EDGE_CURVE('',#9127,#9128,#2650,.T.);
#11558=EDGE_CURVE('',#8238,#9128,#1332,.T.);
#11559=EDGE_CURVE('',#9127,#8236,#1333,.T.);
#11560=EDGE_CURVE('',#9129,#8232,#1334,.T.);
#11561=EDGE_CURVE('',#8237,#9129,#1335,.T.);
#11562=EDGE_CURVE('',#9130,#8239,#1336,.T.);
#11563=EDGE_CURVE('',#8257,#9130,#1337,.T.);
#11564=EDGE_CURVE('',#9131,#8258,#1338,.T.);
#11565=EDGE_CURVE('',#9061,#9131,#1339,.T.);
#11566=EDGE_CURVE('',#9132,#8263,#1402,.T.);
#11567=EDGE_CURVE('',#9133,#9132,#1340,.T.);
#11568=EDGE_CURVE('',#8233,#9133,#1341,.T.);
#11569=EDGE_CURVE('',#9134,#9135,#2651,.T.);
#11570=EDGE_CURVE('',#9132,#9134,#1403,.T.);
#11571=EDGE_CURVE('',#9135,#8259,#2652,.T.);
#11572=EDGE_CURVE('',#9136,#9135,#7612,.T.);
#11573=EDGE_CURVE('',#9134,#9136,#1342,.T.);
#11574=EDGE_CURVE('',#9137,#9138,#7613,.T.);
#11575=EDGE_CURVE('',#9136,#9137,#2653,.T.);
#11576=EDGE_CURVE('',#9138,#8260,#2654,.T.);
#11577=EDGE_CURVE('',#9139,#9138,#2655,.T.);
#11578=EDGE_CURVE('',#9137,#9139,#1343,.T.);
#11579=EDGE_CURVE('',#9139,#8225,#1404,.T.);
#11580=EDGE_CURVE('',#9140,#8220,#1344,.T.);
#11581=EDGE_CURVE('',#8231,#9140,#1345,.T.);
#11582=EDGE_CURVE('',#9141,#8230,#1346,.T.);
#11583=EDGE_CURVE('',#8222,#9141,#1347,.T.);
#11584=EDGE_CURVE('',#9142,#8216,#1348,.T.);
#11585=EDGE_CURVE('',#8221,#9142,#1349,.T.);
#11586=EDGE_CURVE('',#9143,#8223,#1350,.T.);
#11587=EDGE_CURVE('',#8218,#9143,#1351,.T.);
#11588=EDGE_CURVE('',#9144,#8219,#1352,.T.);
#11589=EDGE_CURVE('',#9144,#9145,#2656,.T.);
#11590=EDGE_CURVE('',#8217,#9145,#1353,.T.);
#11591=EDGE_CURVE('',#9118,#9107,#2657,.T.);
#11592=EDGE_CURVE('',#9145,#9114,#2658,.T.);
#11593=EDGE_CURVE('',#9101,#9144,#2659,.T.);
#11594=EDGE_CURVE('',#9146,#9115,#2660,.T.);
#11595=EDGE_CURVE('',#9114,#9146,#7614,.T.);
#11596=EDGE_CURVE('',#9147,#9148,#1354,.T.);
#11597=EDGE_CURVE('',#9149,#9147,#1355,.T.);
#11598=EDGE_CURVE('',#9149,#9148,#1356,.T.);
#11599=EDGE_CURVE('',#9150,#9151,#2661,.T.);
#11600=EDGE_CURVE('',#9152,#9150,#2662,.T.);
#11601=EDGE_CURVE('',#9153,#9152,#2663,.T.);
#11602=EDGE_CURVE('',#9153,#9154,#7615,.T.);
#11603=EDGE_CURVE('',#9128,#9154,#2664,.T.);
#11604=EDGE_CURVE('',#9155,#9127,#2665,.T.);
#11605=EDGE_CURVE('',#9155,#9151,#7616,.T.);
#11606=EDGE_CURVE('',#9156,#9157,#2666,.T.);
#11607=EDGE_CURVE('',#9154,#9156,#7617,.T.);
#11608=EDGE_CURVE('',#9154,#9157,#2667,.T.);
#11609=EDGE_CURVE('',#9158,#9153,#2668,.T.);
#11610=EDGE_CURVE('',#9157,#9158,#7618,.T.);
#11611=EDGE_CURVE('',#9159,#9152,#7619,.T.);
#11612=EDGE_CURVE('',#9159,#9160,#2669,.T.);
#11613=EDGE_CURVE('',#9158,#9160,#2670,.T.);
#11614=EDGE_CURVE('',#9161,#9156,#2671,.T.);
#11615=EDGE_CURVE('',#9162,#9161,#1405,.T.);
#11616=EDGE_CURVE('',#9147,#9162,#2672,.T.);
#11617=EDGE_CURVE('',#9148,#9102,#2673,.T.);
#11618=EDGE_CURVE('',#9066,#9163,#2674,.T.);
#11619=EDGE_CURVE('',#9164,#9163,#2675,.T.);
#11620=EDGE_CURVE('',#9164,#9067,#2676,.T.);
#11621=EDGE_CURVE('',#9065,#9165,#2677,.T.);
#11622=EDGE_CURVE('',#9163,#9165,#2678,.T.);
#11623=EDGE_CURVE('',#9064,#9166,#2679,.T.);
#11624=EDGE_CURVE('',#9165,#9166,#2680,.T.);
#11625=EDGE_CURVE('',#9063,#9167,#2681,.T.);
#11626=EDGE_CURVE('',#9166,#9167,#2682,.T.);
#11627=EDGE_CURVE('',#9062,#9168,#2683,.T.);
#11628=EDGE_CURVE('',#9167,#9168,#2684,.T.);
#11629=EDGE_CURVE('',#9168,#9164,#2685,.T.);
#11630=EDGE_CURVE('',#9169,#9161,#1357,.T.);
#11631=EDGE_CURVE('',#9162,#9169,#1358,.T.);
#11632=EDGE_CURVE('',#9170,#9155,#2686,.T.);
#11633=EDGE_CURVE('',#9171,#9155,#7620,.T.);
#11634=EDGE_CURVE('',#9171,#9170,#2687,.T.);
#11635=EDGE_CURVE('',#9151,#9172,#2688,.T.);
#11636=EDGE_CURVE('',#9170,#9172,#7621,.T.);
#11637=EDGE_CURVE('',#9172,#9173,#2689,.T.);
#11638=EDGE_CURVE('',#9173,#9174,#2690,.T.);
#11639=EDGE_CURVE('',#9150,#9174,#7622,.T.);
#11640=EDGE_CURVE('',#9072,#9175,#2691,.T.);
#11641=EDGE_CURVE('',#9175,#9176,#2692,.T.);
#11642=EDGE_CURVE('',#9176,#9073,#2693,.T.);
#11643=EDGE_CURVE('',#9176,#9177,#2694,.T.);
#11644=EDGE_CURVE('',#9177,#9068,#2695,.T.);
#11645=EDGE_CURVE('',#9177,#9178,#2696,.T.);
#11646=EDGE_CURVE('',#9178,#9069,#2697,.T.);
#11647=EDGE_CURVE('',#9178,#9179,#2698,.T.);
#11648=EDGE_CURVE('',#9179,#9070,#2699,.T.);
#11649=EDGE_CURVE('',#9179,#9180,#2700,.T.);
#11650=EDGE_CURVE('',#9180,#9071,#2701,.T.);
#11651=EDGE_CURVE('',#9180,#9175,#2702,.T.);
#11652=EDGE_CURVE('',#9181,#9077,#2703,.T.);
#11653=EDGE_CURVE('',#9076,#9182,#2704,.T.);
#11654=EDGE_CURVE('',#9181,#9182,#2705,.T.);
#11655=EDGE_CURVE('',#9075,#9183,#2706,.T.);
#11656=EDGE_CURVE('',#9182,#9183,#2707,.T.);
#11657=EDGE_CURVE('',#9074,#9184,#2708,.T.);
#11658=EDGE_CURVE('',#9183,#9184,#2709,.T.);
#11659=EDGE_CURVE('',#9079,#9185,#2710,.T.);
#11660=EDGE_CURVE('',#9184,#9185,#2711,.T.);
#11661=EDGE_CURVE('',#9078,#9186,#2712,.T.);
#11662=EDGE_CURVE('',#9185,#9186,#2713,.T.);
#11663=EDGE_CURVE('',#9186,#9181,#2714,.T.);
#11664=EDGE_CURVE('',#9187,#9188,#2715,.T.);
#11665=EDGE_CURVE('',#9188,#9189,#2716,.T.);
#11666=EDGE_CURVE('',#9189,#9190,#2717,.T.);
#11667=EDGE_CURVE('',#9190,#9191,#2718,.T.);
#11668=EDGE_CURVE('',#9191,#9192,#2719,.T.);
#11669=EDGE_CURVE('',#9192,#9187,#2720,.T.);
#11670=EDGE_CURVE('',#9193,#9194,#2721,.T.);
#11671=EDGE_CURVE('',#9195,#9193,#2722,.T.);
#11672=EDGE_CURVE('',#9196,#9195,#2723,.T.);
#11673=EDGE_CURVE('',#9197,#9196,#2724,.T.);
#11674=EDGE_CURVE('',#9198,#9197,#2725,.T.);
#11675=EDGE_CURVE('',#9194,#9198,#2726,.T.);
#11676=EDGE_CURVE('',#9199,#9200,#2727,.T.);
#11677=EDGE_CURVE('',#9193,#9200,#2728,.T.);
#11678=EDGE_CURVE('',#9199,#9194,#2729,.T.);
#11679=EDGE_CURVE('',#9200,#9201,#2730,.T.);
#11680=EDGE_CURVE('',#9202,#9199,#2731,.T.);
#11681=EDGE_CURVE('',#9203,#9202,#2732,.T.);
#11682=EDGE_CURVE('',#9204,#9203,#2733,.T.);
#11683=EDGE_CURVE('',#9201,#9204,#2734,.T.);
#11684=EDGE_CURVE('',#9205,#9206,#2735,.T.);
#11685=EDGE_CURVE('',#9204,#9206,#2736,.T.);
#11686=EDGE_CURVE('',#9205,#9203,#2737,.T.);
#11687=EDGE_CURVE('',#9207,#9082,#2738,.T.);
#11688=EDGE_CURVE('',#9087,#9208,#2739,.T.);
#11689=EDGE_CURVE('',#9207,#9208,#2740,.T.);
#11690=EDGE_CURVE('',#9086,#9209,#2741,.T.);
#11691=EDGE_CURVE('',#9208,#9209,#2742,.T.);
#11692=EDGE_CURVE('',#9085,#9210,#2743,.T.);
#11693=EDGE_CURVE('',#9209,#9210,#2744,.T.);
#11694=EDGE_CURVE('',#9084,#9211,#2745,.T.);
#11695=EDGE_CURVE('',#9210,#9211,#2746,.T.);
#11696=EDGE_CURVE('',#9083,#9212,#2747,.T.);
#11697=EDGE_CURVE('',#9211,#9212,#2748,.T.);
#11698=EDGE_CURVE('',#9212,#9207,#2749,.T.);
#11699=EDGE_CURVE('',#9213,#9214,#7623,.T.);
#11700=EDGE_CURVE('',#9215,#9213,#2750,.T.);
#11701=EDGE_CURVE('',#9215,#9088,#2751,.T.);
#11702=EDGE_CURVE('',#9093,#9216,#2752,.T.);
#11703=EDGE_CURVE('',#9214,#9216,#2753,.T.);
#11704=EDGE_CURVE('',#9092,#9217,#2754,.T.);
#11705=EDGE_CURVE('',#9216,#9217,#2755,.T.);
#11706=EDGE_CURVE('',#9091,#9218,#2756,.T.);
#11707=EDGE_CURVE('',#9217,#9218,#2757,.T.);
#11708=EDGE_CURVE('',#9090,#9219,#2758,.T.);
#11709=EDGE_CURVE('',#9220,#9219,#2759,.T.);
#11710=EDGE_CURVE('',#9221,#9220,#7624,.T.);
#11711=EDGE_CURVE('',#9218,#9221,#2760,.T.);
#11712=EDGE_CURVE('',#9089,#9222,#2761,.T.);
#11713=EDGE_CURVE('',#9219,#9222,#2762,.T.);
#11714=EDGE_CURVE('',#9222,#9215,#2763,.T.);
#11715=EDGE_CURVE('',#9106,#9119,#2764,.T.);
#11716=EDGE_CURVE('',#9223,#9149,#7625,.T.);
#11717=EDGE_CURVE('',#9223,#9105,#2765,.T.);
#11718=EDGE_CURVE('',#9224,#9225,#1359,.T.);
#11719=EDGE_CURVE('',#9226,#9224,#1360,.T.);
#11720=EDGE_CURVE('',#9225,#9226,#1406,.T.);
#11721=EDGE_CURVE('',#9146,#9225,#2766,.T.);
#11722=EDGE_CURVE('',#9120,#9227,#2767,.T.);
#11723=EDGE_CURVE('',#9224,#9227,#7626,.T.);
#11724=EDGE_CURVE('',#9226,#9228,#2768,.T.);
#11725=EDGE_CURVE('',#9229,#9228,#1407,.T.);
#11726=EDGE_CURVE('',#9229,#9171,#2769,.T.);
#11727=EDGE_CURVE('',#9230,#9228,#1361,.T.);
#11728=EDGE_CURVE('',#9230,#9229,#1362,.T.);
#11729=EDGE_CURVE('',#9206,#9231,#2770,.T.);
#11730=EDGE_CURVE('',#9232,#9205,#2771,.T.);
#11731=EDGE_CURVE('',#9231,#9232,#2772,.T.);
#11732=EDGE_CURVE('',#9233,#9234,#7627,.T.);
#11733=EDGE_CURVE('',#9233,#9223,#2773,.T.);
#11734=EDGE_CURVE('',#9234,#9147,#2774,.T.);
#11735=EDGE_CURVE('',#9234,#9235,#2775,.T.);
#11736=EDGE_CURVE('',#9235,#9162,#2776,.T.);
#11737=EDGE_CURVE('',#9174,#9159,#2777,.T.);
#11738=EDGE_CURVE('',#9160,#9236,#2778,.T.);
#11739=EDGE_CURVE('',#9169,#9236,#7628,.T.);
#11740=EDGE_CURVE('',#9235,#9237,#7629,.T.);
#11741=EDGE_CURVE('',#9236,#9237,#2779,.T.);
#11742=EDGE_CURVE('',#9238,#9230,#7630,.T.);
#11743=EDGE_CURVE('',#9238,#9173,#2780,.T.);
#11744=EDGE_CURVE('',#9239,#9187,#2781,.T.);
#11745=EDGE_CURVE('',#9192,#9240,#2782,.T.);
#11746=EDGE_CURVE('',#9239,#9240,#2783,.T.);
#11747=EDGE_CURVE('',#9191,#9241,#2784,.T.);
#11748=EDGE_CURVE('',#9240,#9241,#2785,.T.);
#11749=EDGE_CURVE('',#9190,#9242,#2786,.T.);
#11750=EDGE_CURVE('',#9241,#9242,#2787,.T.);
#11751=EDGE_CURVE('',#9189,#9243,#2788,.T.);
#11752=EDGE_CURVE('',#9242,#9243,#2789,.T.);
#11753=EDGE_CURVE('',#9188,#9244,#2790,.T.);
#11754=EDGE_CURVE('',#9243,#9244,#2791,.T.);
#11755=EDGE_CURVE('',#9244,#9239,#2792,.T.);
#11756=EDGE_CURVE('',#9232,#9202,#2793,.T.);
#11757=EDGE_CURVE('',#9202,#9198,#2794,.T.);
#11758=EDGE_CURVE('',#9245,#9246,#2795,.T.);
#11759=EDGE_CURVE('',#9198,#9245,#2796,.T.);
#11760=EDGE_CURVE('',#9246,#9197,#2797,.T.);
#11761=EDGE_CURVE('',#9246,#9247,#2798,.T.);
#11762=EDGE_CURVE('',#9247,#9196,#2799,.T.);
#11763=EDGE_CURVE('',#9247,#9248,#2800,.T.);
#11764=EDGE_CURVE('',#9248,#9195,#2801,.T.);
#11765=EDGE_CURVE('',#9195,#9201,#2802,.T.);
#11766=EDGE_CURVE('',#9201,#9231,#2803,.T.);
#11767=EDGE_CURVE('',#9221,#9214,#2804,.T.);
#11768=EDGE_CURVE('',#9213,#8203,#2805,.T.);
#11769=EDGE_CURVE('',#8202,#9220,#2806,.T.);
#11770=EDGE_CURVE('',#9249,#9250,#2807,.T.);
#11771=EDGE_CURVE('',#9249,#9250,#7631,.T.);
#11772=EDGE_CURVE('',#9251,#9252,#2808,.T.);
#11773=EDGE_CURVE('',#9251,#9252,#7632,.T.);
#11774=EDGE_CURVE('',#8211,#8208,#2809,.T.);
#11775=EDGE_CURVE('',#9253,#9233,#2810,.T.);
#11776=EDGE_CURVE('',#9227,#9253,#2811,.T.);
#11777=EDGE_CURVE('',#9254,#9255,#7633,.T.);
#11778=EDGE_CURVE('',#9255,#9226,#2812,.T.);
#11779=EDGE_CURVE('',#9254,#9253,#7634,.T.);
#11780=EDGE_CURVE('',#9228,#9256,#2813,.T.);
#11781=EDGE_CURVE('',#9255,#9256,#2814,.T.);
#11782=EDGE_CURVE('',#9257,#9258,#7635,.T.);
#11783=EDGE_CURVE('',#9257,#9238,#2815,.T.);
#11784=EDGE_CURVE('',#9256,#9258,#7636,.T.);
#11785=EDGE_CURVE('',#9231,#9237,#2816,.T.);
#11786=EDGE_CURVE('',#9233,#9232,#2817,.T.);
#11787=EDGE_CURVE('',#9237,#9257,#2818,.T.);
#11788=EDGE_CURVE('',#9259,#9260,#2819,.T.);
#11789=EDGE_CURVE('',#9259,#9260,#7637,.T.);
#11790=EDGE_CURVE('',#9261,#9262,#2820,.T.);
#11791=EDGE_CURVE('',#9261,#9262,#7638,.T.);
#11792=EDGE_CURVE('',#8194,#9263,#7639,.T.);
#11793=EDGE_CURVE('',#8190,#9263,#7640,.T.);
#11794=EDGE_CURVE('',#9264,#8188,#7641,.T.);
#11795=EDGE_CURVE('',#9265,#8193,#7642,.T.);
#11796=EDGE_CURVE('',#9264,#9265,#1363,.T.);
#11797=EDGE_CURVE('',#9266,#9264,#7643,.T.);
#11798=EDGE_CURVE('',#9267,#9266,#7644,.T.);
#11799=EDGE_CURVE('',#9268,#9267,#7645,.T.);
#11800=EDGE_CURVE('',#9269,#9268,#7646,.T.);
#11801=EDGE_CURVE('',#9269,#8189,#7647,.T.);
#11802=EDGE_CURVE('',#9263,#9269,#1364,.T.);
#11803=EDGE_CURVE('',#9265,#8184,#7648,.T.);
#11804=EDGE_CURVE('',#9270,#9271,#2821,.T.);
#11805=EDGE_CURVE('',#9232,#9270,#2822,.T.);
#11806=EDGE_CURVE('',#9272,#9232,#2823,.T.);
#11807=EDGE_CURVE('',#9273,#9272,#2824,.T.);
#11808=EDGE_CURVE('',#9274,#9273,#2825,.T.);
#11809=EDGE_CURVE('',#9271,#9274,#2826,.T.);
#11810=EDGE_CURVE('',#9202,#9275,#2827,.T.);
#11811=EDGE_CURVE('',#9272,#9275,#2828,.T.);
#11812=EDGE_CURVE('',#9276,#9202,#2829,.T.);
#11813=EDGE_CURVE('',#9277,#9276,#2830,.T.);
#11814=EDGE_CURVE('',#9275,#9277,#2831,.T.);
#11815=EDGE_CURVE('',#9278,#9198,#2832,.T.);
#11816=EDGE_CURVE('',#9276,#9278,#2833,.T.);
#11817=EDGE_CURVE('',#9278,#9279,#2834,.T.);
#11818=EDGE_CURVE('',#9280,#9198,#2835,.T.);
#11819=EDGE_CURVE('',#9279,#9280,#2836,.T.);
#11820=EDGE_CURVE('',#9281,#9245,#2837,.T.);
#11821=EDGE_CURVE('',#9280,#9281,#2838,.T.);
#11822=EDGE_CURVE('',#9282,#9283,#2839,.T.);
#11823=EDGE_CURVE('',#9284,#9282,#2840,.T.);
#11824=EDGE_CURVE('',#9285,#9284,#2841,.T.);
#11825=EDGE_CURVE('',#9286,#9285,#2842,.T.);
#11826=EDGE_CURVE('',#9287,#9286,#2843,.T.);
#11827=EDGE_CURVE('',#9281,#9287,#2844,.T.);
#11828=EDGE_CURVE('',#9288,#9248,#2845,.T.);
#11829=EDGE_CURVE('',#9289,#9288,#2846,.T.);
#11830=EDGE_CURVE('',#9290,#9289,#2847,.T.);
#11831=EDGE_CURVE('',#9283,#9290,#2848,.T.);
#11832=EDGE_CURVE('',#9291,#9195,#2849,.T.);
#11833=EDGE_CURVE('',#9288,#9291,#2850,.T.);
#11834=EDGE_CURVE('',#9292,#9293,#2851,.T.);
#11835=EDGE_CURVE('',#9291,#9292,#2852,.T.);
#11836=EDGE_CURVE('',#9293,#9195,#2853,.T.);
#11837=EDGE_CURVE('',#9201,#9294,#2854,.T.);
#11838=EDGE_CURVE('',#9293,#9294,#2855,.T.);
#11839=EDGE_CURVE('',#9295,#9296,#2856,.T.);
#11840=EDGE_CURVE('',#9294,#9295,#2857,.T.);
#11841=EDGE_CURVE('',#9296,#9201,#2858,.T.);
#11842=EDGE_CURVE('',#9231,#9297,#2859,.T.);
#11843=EDGE_CURVE('',#9296,#9297,#2860,.T.);
#11844=EDGE_CURVE('',#9298,#9299,#2861,.T.);
#11845=EDGE_CURVE('',#9297,#9298,#2862,.T.);
#11846=EDGE_CURVE('',#9300,#9231,#2863,.T.);
#11847=EDGE_CURVE('',#9301,#9300,#2864,.T.);
#11848=EDGE_CURVE('',#9299,#9301,#2865,.T.);
#11849=EDGE_CURVE('',#9302,#9303,#2866,.T.);
#11850=EDGE_CURVE('',#9303,#8201,#2867,.T.);
#11851=EDGE_CURVE('',#8200,#9302,#2868,.T.);
#11852=EDGE_CURVE('',#9303,#9304,#7649,.T.);
#11853=EDGE_CURVE('',#9260,#9304,#2869,.T.);
#11854=EDGE_CURVE('',#8204,#9259,#2870,.T.);
#11855=EDGE_CURVE('',#9305,#9306,#7650,.T.);
#11856=EDGE_CURVE('',#9250,#9306,#2871,.T.);
#11857=EDGE_CURVE('',#9305,#9249,#2872,.T.);
#11858=EDGE_CURVE('',#9307,#9308,#7651,.T.);
#11859=EDGE_CURVE('',#9252,#9308,#2873,.T.);
#11860=EDGE_CURVE('',#9307,#9251,#2874,.T.);
#11861=EDGE_CURVE('',#9308,#9309,#2875,.T.);
#11862=EDGE_CURVE('',#8206,#9309,#2876,.T.);
#11863=EDGE_CURVE('',#9270,#8207,#2877,.T.);
#11864=EDGE_CURVE('',#9310,#9271,#2878,.T.);
#11865=EDGE_CURVE('',#9310,#9305,#2879,.T.);
#11866=EDGE_CURVE('',#9306,#9307,#2880,.T.);
#11867=EDGE_CURVE('',#9309,#9311,#2881,.T.);
#11868=EDGE_CURVE('',#9253,#9311,#2882,.T.);
#11869=EDGE_CURVE('',#9311,#9254,#2883,.T.);
#11870=EDGE_CURVE('',#9254,#9258,#2884,.T.);
#11871=EDGE_CURVE('',#9258,#9312,#2885,.T.);
#11872=EDGE_CURVE('',#9257,#9312,#2886,.T.);
#11873=EDGE_CURVE('',#9312,#9313,#2887,.T.);
#11874=EDGE_CURVE('',#9300,#9313,#2888,.T.);
#11875=EDGE_CURVE('',#9262,#8205,#2889,.T.);
#11876=EDGE_CURVE('',#9304,#9314,#2890,.T.);
#11877=EDGE_CURVE('',#9301,#9314,#2891,.T.);
#11878=EDGE_CURVE('',#9313,#9315,#2892,.T.);
#11879=EDGE_CURVE('',#9315,#9261,#2893,.T.);
#11880=EDGE_CURVE('',#9315,#9302,#7652,.T.);
#11881=EDGE_CURVE('',#9266,#9316,#1365,.T.);
#11882=EDGE_CURVE('',#8187,#9316,#7653,.T.);
#11883=EDGE_CURVE('',#9316,#9317,#7654,.T.);
#11884=EDGE_CURVE('',#9267,#9317,#1366,.T.);
#11885=EDGE_CURVE('',#9268,#9318,#1367,.T.);
#11886=EDGE_CURVE('',#9317,#9318,#7655,.T.);
#11887=EDGE_CURVE('',#9318,#8195,#7656,.T.);
#11888=EDGE_CURVE('',#9319,#9320,#2894,.T.);
#11889=EDGE_CURVE('',#9321,#9320,#2895,.T.);
#11890=EDGE_CURVE('',#9321,#9310,#2896,.T.);
#11891=EDGE_CURVE('',#9319,#9274,#2897,.T.);
#11892=EDGE_CURVE('',#9320,#9322,#2898,.T.);
#11893=EDGE_CURVE('',#9323,#9322,#2899,.T.);
#11894=EDGE_CURVE('',#9323,#9321,#2900,.T.);
#11895=EDGE_CURVE('',#9324,#9319,#2901,.T.);
#11896=EDGE_CURVE('',#9324,#9273,#2902,.T.);
#11897=EDGE_CURVE('',#9273,#9277,#2903,.T.);
#11898=EDGE_CURVE('',#9277,#9279,#2904,.T.);
#11899=EDGE_CURVE('',#8181,#9287,#2905,.T.);
#11900=EDGE_CURVE('',#9279,#8180,#2906,.T.);
#11901=EDGE_CURVE('',#9325,#9326,#2907,.T.);
#11902=EDGE_CURVE('',#9287,#9325,#2908,.T.);
#11903=EDGE_CURVE('',#9326,#9286,#2909,.T.);
#11904=EDGE_CURVE('',#9326,#9327,#2910,.T.);
#11905=EDGE_CURVE('',#9327,#9285,#2911,.T.);
#11906=EDGE_CURVE('',#9327,#9328,#2912,.T.);
#11907=EDGE_CURVE('',#9328,#9284,#2913,.T.);
#11908=EDGE_CURVE('',#9329,#9282,#2914,.T.);
#11909=EDGE_CURVE('',#9330,#9329,#2915,.T.);
#11910=EDGE_CURVE('',#9284,#9330,#2916,.T.);
#11911=EDGE_CURVE('',#9331,#9332,#2917,.T.);
#11912=EDGE_CURVE('',#9282,#9331,#2918,.T.);
#11913=EDGE_CURVE('',#9332,#9283,#2919,.T.);
#11914=EDGE_CURVE('',#9332,#9333,#2920,.T.);
#11915=EDGE_CURVE('',#9333,#9290,#2921,.T.);
#11916=EDGE_CURVE('',#9333,#9334,#2922,.T.);
#11917=EDGE_CURVE('',#9334,#9289,#2923,.T.);
#11918=EDGE_CURVE('',#9289,#9292,#2924,.T.);
#11919=EDGE_CURVE('',#9292,#9295,#2925,.T.);
#11920=EDGE_CURVE('',#9295,#9298,#2926,.T.);
#11921=EDGE_CURVE('',#9335,#9336,#2927,.T.);
#11922=EDGE_CURVE('',#9299,#9336,#2928,.T.);
#11923=EDGE_CURVE('',#9314,#9337,#2929,.T.);
#11924=EDGE_CURVE('',#9335,#9337,#2930,.T.);
#11925=EDGE_CURVE('',#9336,#9338,#2931,.T.);
#11926=EDGE_CURVE('',#9298,#9338,#2932,.T.);
#11927=EDGE_CURVE('',#9339,#9335,#2933,.T.);
#11928=EDGE_CURVE('',#9337,#9340,#2934,.T.);
#11929=EDGE_CURVE('',#9339,#9340,#2935,.T.);
#11930=EDGE_CURVE('',#9341,#9323,#2936,.T.);
#11931=EDGE_CURVE('',#9342,#9341,#2937,.T.);
#11932=EDGE_CURVE('',#9340,#9342,#2938,.T.);
#11933=EDGE_CURVE('',#9322,#9343,#2939,.T.);
#11934=EDGE_CURVE('',#9341,#9343,#2940,.T.);
#11935=EDGE_CURVE('',#9344,#9324,#2941,.T.);
#11936=EDGE_CURVE('',#9343,#9344,#2942,.T.);
#11937=EDGE_CURVE('',#9345,#9325,#2943,.T.);
#11938=EDGE_CURVE('',#9344,#9345,#2944,.T.);
#11939=EDGE_CURVE('',#9346,#9328,#2945,.T.);
#11940=EDGE_CURVE('',#9345,#9346,#2946,.T.);
#11941=EDGE_CURVE('',#9347,#9330,#2947,.T.);
#11942=EDGE_CURVE('',#9346,#9347,#2948,.T.);
#11943=EDGE_CURVE('',#9348,#9329,#2949,.T.);
#11944=EDGE_CURVE('',#9347,#9348,#2950,.T.);
#11945=EDGE_CURVE('',#9349,#9331,#2951,.T.);
#11946=EDGE_CURVE('',#9348,#9349,#2952,.T.);
#11947=EDGE_CURVE('',#9350,#9334,#2953,.T.);
#11948=EDGE_CURVE('',#9349,#9350,#2954,.T.);
#11949=EDGE_CURVE('',#9338,#9351,#2955,.T.);
#11950=EDGE_CURVE('',#9350,#9351,#2956,.T.);
#11951=EDGE_CURVE('',#9352,#9339,#2957,.T.);
#11952=EDGE_CURVE('',#9351,#9352,#2958,.T.);
#11953=EDGE_CURVE('',#9352,#9342,#2959,.T.);
#11954=EDGE_CURVE('',#9353,#9354,#7657,.T.);
#11955=EDGE_CURVE('',#9354,#9353,#7658,.T.);
#11956=EDGE_CURVE('',#9354,#9355,#7659,.T.);
#11957=EDGE_CURVE('',#9355,#9355,#7660,.T.);
#11958=EDGE_CURVE('',#9356,#9357,#7661,.T.);
#11959=EDGE_CURVE('',#9358,#9356,#7662,.T.);
#11960=EDGE_CURVE('',#9359,#9358,#7663,.T.);
#11961=EDGE_CURVE('',#9359,#9360,#2960,.T.);
#11962=EDGE_CURVE('',#9360,#9360,#7664,.T.);
#11963=EDGE_CURVE('',#9361,#9359,#7665,.T.);
#11964=EDGE_CURVE('',#9362,#9361,#7666,.T.);
#11965=EDGE_CURVE('',#9357,#9362,#7667,.T.);
#11966=EDGE_CURVE('',#9363,#9363,#7668,.T.);
#11967=EDGE_CURVE('',#9363,#9364,#2961,.T.);
#11968=EDGE_CURVE('',#9364,#9364,#7669,.T.);
#11969=EDGE_CURVE('',#9353,#9363,#2962,.T.);
#11970=EDGE_CURVE('',#9365,#9361,#2963,.T.);
#11971=EDGE_CURVE('',#9359,#9365,#2964,.T.);
#11972=EDGE_CURVE('',#9361,#9366,#2965,.T.);
#11973=EDGE_CURVE('',#9366,#9362,#2966,.T.);
#11974=EDGE_CURVE('',#9362,#9367,#2967,.T.);
#11975=EDGE_CURVE('',#9367,#9357,#2968,.T.);
#11976=EDGE_CURVE('',#9357,#9368,#2969,.T.);
#11977=EDGE_CURVE('',#9368,#9356,#2970,.T.);
#11978=EDGE_CURVE('',#9356,#9369,#2971,.T.);
#11979=EDGE_CURVE('',#9369,#9358,#2972,.T.);
#11980=EDGE_CURVE('',#9358,#9370,#2973,.T.);
#11981=EDGE_CURVE('',#9370,#9359,#2974,.T.);
#11982=EDGE_CURVE('',#9371,#9372,#7670,.T.);
#11983=EDGE_CURVE('',#9373,#9371,#7671,.T.);
#11984=EDGE_CURVE('',#9374,#9373,#7672,.T.);
#11985=EDGE_CURVE('',#9375,#9374,#7673,.T.);
#11986=EDGE_CURVE('',#9375,#9376,#7674,.T.);
#11987=EDGE_CURVE('',#9372,#9376,#7675,.T.);
#11988=EDGE_CURVE('',#9376,#9377,#113,.T.);
#11989=EDGE_CURVE('',#9377,#9372,#114,.T.);
#11990=EDGE_CURVE('',#9375,#9378,#115,.T.);
#11991=EDGE_CURVE('',#9378,#9376,#116,.T.);
#11992=EDGE_CURVE('',#9379,#9375,#117,.T.);
#11993=EDGE_CURVE('',#9374,#9379,#118,.T.);
#11994=EDGE_CURVE('',#9380,#9374,#119,.T.);
#11995=EDGE_CURVE('',#9373,#9380,#120,.T.);
#11996=EDGE_CURVE('',#9372,#9381,#121,.T.);
#11997=EDGE_CURVE('',#9381,#9371,#122,.T.);
#11998=EDGE_CURVE('',#9382,#9373,#123,.T.);
#11999=EDGE_CURVE('',#9371,#9382,#124,.T.);
#12000=EDGE_CURVE('',#9370,#9382,#2975,.T.);
#12001=EDGE_CURVE('',#9365,#9381,#2976,.T.);
#12002=EDGE_CURVE('',#9369,#9380,#2977,.T.);
#12003=EDGE_CURVE('',#9368,#9379,#2978,.T.);
#12004=EDGE_CURVE('',#9367,#9378,#2979,.T.);
#12005=EDGE_CURVE('',#9366,#9377,#2980,.T.);
#12006=ORIENTED_EDGE('',*,*,#9383,.F.);
#12007=ORIENTED_EDGE('',*,*,#9384,.T.);
#12008=ORIENTED_EDGE('',*,*,#9385,.F.);
#12009=ORIENTED_EDGE('',*,*,#9384,.F.);
#12010=ORIENTED_EDGE('',*,*,#9386,.F.);
#12011=ORIENTED_EDGE('',*,*,#9387,.F.);
#12012=ORIENTED_EDGE('',*,*,#9388,.T.);
#12013=ORIENTED_EDGE('',*,*,#9389,.F.);
#12014=ORIENTED_EDGE('',*,*,#9388,.F.);
#12015=ORIENTED_EDGE('',*,*,#9390,.T.);
#12016=ORIENTED_EDGE('',*,*,#9391,.T.);
#12017=ORIENTED_EDGE('',*,*,#9392,.F.);
#12018=ORIENTED_EDGE('',*,*,#9393,.F.);
#12019=ORIENTED_EDGE('',*,*,#9394,.T.);
#12020=ORIENTED_EDGE('',*,*,#9395,.T.);
#12021=ORIENTED_EDGE('',*,*,#9396,.F.);
#12022=ORIENTED_EDGE('',*,*,#9397,.F.);
#12023=ORIENTED_EDGE('',*,*,#9398,.T.);
#12024=ORIENTED_EDGE('',*,*,#9399,.T.);
#12025=ORIENTED_EDGE('',*,*,#9400,.F.);
#12026=ORIENTED_EDGE('',*,*,#9401,.F.);
#12027=ORIENTED_EDGE('',*,*,#9402,.T.);
#12028=ORIENTED_EDGE('',*,*,#9403,.T.);
#12029=ORIENTED_EDGE('',*,*,#9404,.F.);
#12030=ORIENTED_EDGE('',*,*,#9405,.F.);
#12031=ORIENTED_EDGE('',*,*,#9406,.T.);
#12032=ORIENTED_EDGE('',*,*,#9407,.T.);
#12033=ORIENTED_EDGE('',*,*,#9408,.F.);
#12034=ORIENTED_EDGE('',*,*,#9407,.F.);
#12035=ORIENTED_EDGE('',*,*,#9409,.T.);
#12036=ORIENTED_EDGE('',*,*,#9410,.T.);
#12037=ORIENTED_EDGE('',*,*,#9411,.F.);
#12038=ORIENTED_EDGE('',*,*,#9412,.F.);
#12039=ORIENTED_EDGE('',*,*,#9413,.T.);
#12040=ORIENTED_EDGE('',*,*,#9414,.T.);
#12041=ORIENTED_EDGE('',*,*,#9415,.F.);
#12042=ORIENTED_EDGE('',*,*,#9416,.F.);
#12043=ORIENTED_EDGE('',*,*,#9417,.T.);
#12044=ORIENTED_EDGE('',*,*,#9418,.T.);
#12045=ORIENTED_EDGE('',*,*,#9419,.F.);
#12046=ORIENTED_EDGE('',*,*,#9420,.F.);
#12047=ORIENTED_EDGE('',*,*,#9421,.T.);
#12048=ORIENTED_EDGE('',*,*,#9422,.T.);
#12049=ORIENTED_EDGE('',*,*,#9423,.F.);
#12050=ORIENTED_EDGE('',*,*,#9424,.F.);
#12051=ORIENTED_EDGE('',*,*,#9425,.T.);
#12052=ORIENTED_EDGE('',*,*,#9426,.T.);
#12053=ORIENTED_EDGE('',*,*,#9427,.F.);
#12054=ORIENTED_EDGE('',*,*,#9428,.F.);
#12055=ORIENTED_EDGE('',*,*,#9429,.T.);
#12056=ORIENTED_EDGE('',*,*,#9430,.T.);
#12057=ORIENTED_EDGE('',*,*,#9431,.F.);
#12058=ORIENTED_EDGE('',*,*,#9430,.F.);
#12059=ORIENTED_EDGE('',*,*,#9432,.T.);
#12060=ORIENTED_EDGE('',*,*,#9433,.T.);
#12061=ORIENTED_EDGE('',*,*,#9434,.F.);
#12062=ORIENTED_EDGE('',*,*,#9433,.F.);
#12063=ORIENTED_EDGE('',*,*,#9435,.T.);
#12064=ORIENTED_EDGE('',*,*,#9436,.T.);
#12065=ORIENTED_EDGE('',*,*,#9437,.F.);
#12066=ORIENTED_EDGE('',*,*,#9436,.F.);
#12067=ORIENTED_EDGE('',*,*,#9438,.T.);
#12068=ORIENTED_EDGE('',*,*,#9439,.T.);
#12069=ORIENTED_EDGE('',*,*,#9440,.F.);
#12070=ORIENTED_EDGE('',*,*,#9439,.F.);
#12071=ORIENTED_EDGE('',*,*,#9441,.T.);
#12072=ORIENTED_EDGE('',*,*,#9442,.T.);
#12073=ORIENTED_EDGE('',*,*,#9443,.F.);
#12074=ORIENTED_EDGE('',*,*,#9442,.F.);
#12075=ORIENTED_EDGE('',*,*,#9444,.T.);
#12076=ORIENTED_EDGE('',*,*,#9445,.T.);
#12077=ORIENTED_EDGE('',*,*,#9446,.F.);
#12078=ORIENTED_EDGE('',*,*,#9445,.F.);
#12079=ORIENTED_EDGE('',*,*,#9447,.T.);
#12080=ORIENTED_EDGE('',*,*,#9448,.T.);
#12081=ORIENTED_EDGE('',*,*,#9449,.F.);
#12082=ORIENTED_EDGE('',*,*,#9448,.F.);
#12083=ORIENTED_EDGE('',*,*,#9450,.T.);
#12084=ORIENTED_EDGE('',*,*,#9451,.T.);
#12085=ORIENTED_EDGE('',*,*,#9452,.F.);
#12086=ORIENTED_EDGE('',*,*,#9451,.F.);
#12087=ORIENTED_EDGE('',*,*,#9453,.F.);
#12088=ORIENTED_EDGE('',*,*,#9454,.T.);
#12089=ORIENTED_EDGE('',*,*,#9455,.T.);
#12090=ORIENTED_EDGE('',*,*,#9454,.F.);
#12091=ORIENTED_EDGE('',*,*,#9456,.F.);
#12092=ORIENTED_EDGE('',*,*,#9457,.T.);
#12093=ORIENTED_EDGE('',*,*,#9458,.T.);
#12094=ORIENTED_EDGE('',*,*,#9457,.F.);
#12095=ORIENTED_EDGE('',*,*,#9459,.F.);
#12096=ORIENTED_EDGE('',*,*,#9460,.T.);
#12097=ORIENTED_EDGE('',*,*,#9461,.T.);
#12098=ORIENTED_EDGE('',*,*,#9460,.F.);
#12099=ORIENTED_EDGE('',*,*,#9462,.F.);
#12100=ORIENTED_EDGE('',*,*,#9463,.T.);
#12101=ORIENTED_EDGE('',*,*,#9464,.T.);
#12102=ORIENTED_EDGE('',*,*,#9463,.F.);
#12103=ORIENTED_EDGE('',*,*,#9385,.T.);
#12104=ORIENTED_EDGE('',*,*,#9465,.T.);
#12105=ORIENTED_EDGE('',*,*,#9466,.T.);
#12106=ORIENTED_EDGE('',*,*,#9465,.F.);
#12107=ORIENTED_EDGE('',*,*,#9467,.F.);
#12108=ORIENTED_EDGE('',*,*,#9468,.T.);
#12109=ORIENTED_EDGE('',*,*,#9469,.T.);
#12110=ORIENTED_EDGE('',*,*,#9468,.F.);
#12111=ORIENTED_EDGE('',*,*,#9470,.F.);
#12112=ORIENTED_EDGE('',*,*,#9471,.T.);
#12113=ORIENTED_EDGE('',*,*,#9472,.T.);
#12114=ORIENTED_EDGE('',*,*,#9471,.F.);
#12115=ORIENTED_EDGE('',*,*,#9473,.F.);
#12116=ORIENTED_EDGE('',*,*,#9474,.T.);
#12117=ORIENTED_EDGE('',*,*,#9475,.T.);
#12118=ORIENTED_EDGE('',*,*,#9474,.F.);
#12119=ORIENTED_EDGE('',*,*,#9476,.F.);
#12120=ORIENTED_EDGE('',*,*,#9477,.T.);
#12121=ORIENTED_EDGE('',*,*,#9478,.T.);
#12122=ORIENTED_EDGE('',*,*,#9477,.F.);
#12123=ORIENTED_EDGE('',*,*,#9479,.F.);
#12124=ORIENTED_EDGE('',*,*,#9480,.T.);
#12125=ORIENTED_EDGE('',*,*,#9481,.T.);
#12126=ORIENTED_EDGE('',*,*,#9480,.F.);
#12127=ORIENTED_EDGE('',*,*,#9482,.F.);
#12128=ORIENTED_EDGE('',*,*,#9483,.T.);
#12129=ORIENTED_EDGE('',*,*,#9484,.T.);
#12130=ORIENTED_EDGE('',*,*,#9483,.F.);
#12131=ORIENTED_EDGE('',*,*,#9485,.F.);
#12132=ORIENTED_EDGE('',*,*,#9486,.T.);
#12133=ORIENTED_EDGE('',*,*,#9487,.T.);
#12134=ORIENTED_EDGE('',*,*,#9486,.F.);
#12135=ORIENTED_EDGE('',*,*,#9488,.F.);
#12136=ORIENTED_EDGE('',*,*,#9489,.T.);
#12137=ORIENTED_EDGE('',*,*,#9490,.T.);
#12138=ORIENTED_EDGE('',*,*,#9489,.F.);
#12139=ORIENTED_EDGE('',*,*,#9491,.F.);
#12140=ORIENTED_EDGE('',*,*,#9492,.T.);
#12141=ORIENTED_EDGE('',*,*,#9493,.T.);
#12142=ORIENTED_EDGE('',*,*,#9492,.F.);
#12143=ORIENTED_EDGE('',*,*,#9494,.F.);
#12144=ORIENTED_EDGE('',*,*,#9495,.T.);
#12145=ORIENTED_EDGE('',*,*,#9496,.T.);
#12146=ORIENTED_EDGE('',*,*,#9495,.F.);
#12147=ORIENTED_EDGE('',*,*,#9497,.F.);
#12148=ORIENTED_EDGE('',*,*,#9498,.T.);
#12149=ORIENTED_EDGE('',*,*,#9499,.T.);
#12150=ORIENTED_EDGE('',*,*,#9498,.F.);
#12151=ORIENTED_EDGE('',*,*,#9500,.F.);
#12152=ORIENTED_EDGE('',*,*,#9501,.T.);
#12153=ORIENTED_EDGE('',*,*,#9502,.T.);
#12154=ORIENTED_EDGE('',*,*,#9501,.F.);
#12155=ORIENTED_EDGE('',*,*,#9503,.F.);
#12156=ORIENTED_EDGE('',*,*,#9504,.T.);
#12157=ORIENTED_EDGE('',*,*,#9505,.T.);
#12158=ORIENTED_EDGE('',*,*,#9504,.F.);
#12159=ORIENTED_EDGE('',*,*,#9506,.F.);
#12160=ORIENTED_EDGE('',*,*,#9507,.T.);
#12161=ORIENTED_EDGE('',*,*,#9508,.T.);
#12162=ORIENTED_EDGE('',*,*,#9507,.F.);
#12163=ORIENTED_EDGE('',*,*,#9509,.F.);
#12164=ORIENTED_EDGE('',*,*,#9510,.T.);
#12165=ORIENTED_EDGE('',*,*,#9511,.T.);
#12166=ORIENTED_EDGE('',*,*,#9510,.F.);
#12167=ORIENTED_EDGE('',*,*,#9386,.T.);
#12168=ORIENTED_EDGE('',*,*,#9387,.T.);
#12169=ORIENTED_EDGE('',*,*,#9512,.T.);
#12170=ORIENTED_EDGE('',*,*,#9513,.F.);
#12171=ORIENTED_EDGE('',*,*,#9512,.F.);
#12172=ORIENTED_EDGE('',*,*,#9456,.T.);
#12173=ORIENTED_EDGE('',*,*,#9453,.T.);
#12174=ORIENTED_EDGE('',*,*,#9514,.F.);
#12175=ORIENTED_EDGE('',*,*,#9515,.T.);
#12176=ORIENTED_EDGE('',*,*,#9516,.T.);
#12177=ORIENTED_EDGE('',*,*,#9515,.F.);
#12178=ORIENTED_EDGE('',*,*,#9517,.T.);
#12179=ORIENTED_EDGE('',*,*,#9518,.T.);
#12180=ORIENTED_EDGE('',*,*,#9519,.T.);
#12181=ORIENTED_EDGE('',*,*,#9518,.F.);
#12182=ORIENTED_EDGE('',*,*,#9462,.T.);
#12183=ORIENTED_EDGE('',*,*,#9459,.T.);
#12184=ORIENTED_EDGE('',*,*,#9517,.F.);
#12185=ORIENTED_EDGE('',*,*,#9520,.F.);
#12186=ORIENTED_EDGE('',*,*,#9413,.F.);
#12187=ORIENTED_EDGE('',*,*,#9521,.T.);
#12188=ORIENTED_EDGE('',*,*,#9522,.F.);
#12189=ORIENTED_EDGE('',*,*,#9523,.F.);
#12190=ORIENTED_EDGE('',*,*,#9409,.F.);
#12191=ORIENTED_EDGE('',*,*,#9406,.F.);
#12192=ORIENTED_EDGE('',*,*,#9524,.T.);
#12193=ORIENTED_EDGE('',*,*,#9525,.F.);
#12194=ORIENTED_EDGE('',*,*,#9526,.F.);
#12195=ORIENTED_EDGE('',*,*,#9402,.F.);
#12196=ORIENTED_EDGE('',*,*,#9527,.T.);
#12197=ORIENTED_EDGE('',*,*,#9528,.F.);
#12198=ORIENTED_EDGE('',*,*,#9529,.F.);
#12199=ORIENTED_EDGE('',*,*,#9398,.F.);
#12200=ORIENTED_EDGE('',*,*,#9530,.T.);
#12201=ORIENTED_EDGE('',*,*,#9531,.F.);
#12202=ORIENTED_EDGE('',*,*,#9532,.F.);
#12203=ORIENTED_EDGE('',*,*,#9394,.F.);
#12204=ORIENTED_EDGE('',*,*,#9533,.T.);
#12205=ORIENTED_EDGE('',*,*,#9534,.F.);
#12206=ORIENTED_EDGE('',*,*,#9535,.F.);
#12207=ORIENTED_EDGE('',*,*,#9390,.F.);
#12208=ORIENTED_EDGE('',*,*,#9536,.T.);
#12209=ORIENTED_EDGE('',*,*,#9537,.F.);
#12210=ORIENTED_EDGE('',*,*,#9538,.F.);
#12211=ORIENTED_EDGE('',*,*,#9425,.F.);
#12212=ORIENTED_EDGE('',*,*,#9539,.T.);
#12213=ORIENTED_EDGE('',*,*,#9540,.F.);
#12214=ORIENTED_EDGE('',*,*,#9541,.F.);
#12215=ORIENTED_EDGE('',*,*,#9421,.F.);
#12216=ORIENTED_EDGE('',*,*,#9542,.T.);
#12217=ORIENTED_EDGE('',*,*,#9543,.F.);
#12218=ORIENTED_EDGE('',*,*,#9544,.F.);
#12219=ORIENTED_EDGE('',*,*,#9417,.F.);
#12220=ORIENTED_EDGE('',*,*,#9545,.T.);
#12221=ORIENTED_EDGE('',*,*,#9546,.F.);
#12222=ORIENTED_EDGE('',*,*,#9514,.T.);
#12223=ORIENTED_EDGE('',*,*,#9469,.F.);
#12224=ORIENTED_EDGE('',*,*,#9472,.F.);
#12225=ORIENTED_EDGE('',*,*,#9475,.F.);
#12226=ORIENTED_EDGE('',*,*,#9478,.F.);
#12227=ORIENTED_EDGE('',*,*,#9481,.F.);
#12228=ORIENTED_EDGE('',*,*,#9484,.F.);
#12229=ORIENTED_EDGE('',*,*,#9487,.F.);
#12230=ORIENTED_EDGE('',*,*,#9490,.F.);
#12231=ORIENTED_EDGE('',*,*,#9493,.F.);
#12232=ORIENTED_EDGE('',*,*,#9496,.F.);
#12233=ORIENTED_EDGE('',*,*,#9499,.F.);
#12234=ORIENTED_EDGE('',*,*,#9502,.F.);
#12235=ORIENTED_EDGE('',*,*,#9505,.F.);
#12236=ORIENTED_EDGE('',*,*,#9508,.F.);
#12237=ORIENTED_EDGE('',*,*,#9511,.F.);
#12238=ORIENTED_EDGE('',*,*,#9519,.F.);
#12239=ORIENTED_EDGE('',*,*,#9516,.F.);
#12240=ORIENTED_EDGE('',*,*,#9513,.T.);
#12241=ORIENTED_EDGE('',*,*,#9467,.T.);
#12242=ORIENTED_EDGE('',*,*,#9470,.T.);
#12243=ORIENTED_EDGE('',*,*,#9473,.T.);
#12244=ORIENTED_EDGE('',*,*,#9476,.T.);
#12245=ORIENTED_EDGE('',*,*,#9479,.T.);
#12246=ORIENTED_EDGE('',*,*,#9482,.T.);
#12247=ORIENTED_EDGE('',*,*,#9485,.T.);
#12248=ORIENTED_EDGE('',*,*,#9488,.T.);
#12249=ORIENTED_EDGE('',*,*,#9491,.T.);
#12250=ORIENTED_EDGE('',*,*,#9494,.T.);
#12251=ORIENTED_EDGE('',*,*,#9497,.T.);
#12252=ORIENTED_EDGE('',*,*,#9500,.T.);
#12253=ORIENTED_EDGE('',*,*,#9503,.T.);
#12254=ORIENTED_EDGE('',*,*,#9506,.T.);
#12255=ORIENTED_EDGE('',*,*,#9509,.T.);
#12256=ORIENTED_EDGE('',*,*,#9389,.T.);
#12257=ORIENTED_EDGE('',*,*,#9383,.T.);
#12258=ORIENTED_EDGE('',*,*,#9547,.T.);
#12259=ORIENTED_EDGE('',*,*,#9548,.T.);
#12260=ORIENTED_EDGE('',*,*,#9549,.T.);
#12261=ORIENTED_EDGE('',*,*,#9550,.T.);
#12262=ORIENTED_EDGE('',*,*,#9551,.T.);
#12263=ORIENTED_EDGE('',*,*,#9552,.T.);
#12264=ORIENTED_EDGE('',*,*,#9553,.T.);
#12265=ORIENTED_EDGE('',*,*,#9554,.T.);
#12266=ORIENTED_EDGE('',*,*,#9450,.F.);
#12267=ORIENTED_EDGE('',*,*,#9444,.F.);
#12268=ORIENTED_EDGE('',*,*,#9464,.F.);
#12269=ORIENTED_EDGE('',*,*,#9441,.F.);
#12270=ORIENTED_EDGE('',*,*,#9447,.F.);
#12271=ORIENTED_EDGE('',*,*,#9555,.F.);
#12272=ORIENTED_EDGE('',*,*,#9556,.F.);
#12273=ORIENTED_EDGE('',*,*,#9557,.F.);
#12274=ORIENTED_EDGE('',*,*,#9558,.F.);
#12275=ORIENTED_EDGE('',*,*,#9559,.F.);
#12276=ORIENTED_EDGE('',*,*,#9560,.F.);
#12277=ORIENTED_EDGE('',*,*,#9561,.F.);
#12278=ORIENTED_EDGE('',*,*,#9562,.F.);
#12279=ORIENTED_EDGE('',*,*,#9452,.T.);
#12280=ORIENTED_EDGE('',*,*,#9449,.T.);
#12281=ORIENTED_EDGE('',*,*,#9446,.T.);
#12282=ORIENTED_EDGE('',*,*,#9443,.T.);
#12283=ORIENTED_EDGE('',*,*,#9455,.F.);
#12284=ORIENTED_EDGE('',*,*,#9555,.T.);
#12285=ORIENTED_EDGE('',*,*,#9563,.F.);
#12286=ORIENTED_EDGE('',*,*,#9547,.F.);
#12287=ORIENTED_EDGE('',*,*,#9564,.T.);
#12288=ORIENTED_EDGE('',*,*,#9562,.T.);
#12289=ORIENTED_EDGE('',*,*,#9565,.F.);
#12290=ORIENTED_EDGE('',*,*,#9548,.F.);
#12291=ORIENTED_EDGE('',*,*,#9563,.T.);
#12292=ORIENTED_EDGE('',*,*,#9561,.T.);
#12293=ORIENTED_EDGE('',*,*,#9566,.F.);
#12294=ORIENTED_EDGE('',*,*,#9549,.F.);
#12295=ORIENTED_EDGE('',*,*,#9565,.T.);
#12296=ORIENTED_EDGE('',*,*,#9560,.T.);
#12297=ORIENTED_EDGE('',*,*,#9567,.F.);
#12298=ORIENTED_EDGE('',*,*,#9550,.F.);
#12299=ORIENTED_EDGE('',*,*,#9566,.T.);
#12300=ORIENTED_EDGE('',*,*,#9559,.T.);
#12301=ORIENTED_EDGE('',*,*,#9568,.F.);
#12302=ORIENTED_EDGE('',*,*,#9551,.F.);
#12303=ORIENTED_EDGE('',*,*,#9567,.T.);
#12304=ORIENTED_EDGE('',*,*,#9558,.T.);
#12305=ORIENTED_EDGE('',*,*,#9569,.F.);
#12306=ORIENTED_EDGE('',*,*,#9552,.F.);
#12307=ORIENTED_EDGE('',*,*,#9568,.T.);
#12308=ORIENTED_EDGE('',*,*,#9557,.T.);
#12309=ORIENTED_EDGE('',*,*,#9570,.F.);
#12310=ORIENTED_EDGE('',*,*,#9553,.F.);
#12311=ORIENTED_EDGE('',*,*,#9569,.T.);
#12312=ORIENTED_EDGE('',*,*,#9556,.T.);
#12313=ORIENTED_EDGE('',*,*,#9564,.F.);
#12314=ORIENTED_EDGE('',*,*,#9554,.F.);
#12315=ORIENTED_EDGE('',*,*,#9570,.T.);
#12316=ORIENTED_EDGE('',*,*,#9571,.T.);
#12317=ORIENTED_EDGE('',*,*,#9572,.T.);
#12318=ORIENTED_EDGE('',*,*,#9573,.T.);
#12319=ORIENTED_EDGE('',*,*,#9574,.T.);
#12320=ORIENTED_EDGE('',*,*,#9575,.T.);
#12321=ORIENTED_EDGE('',*,*,#9576,.T.);
#12322=ORIENTED_EDGE('',*,*,#9577,.T.);
#12323=ORIENTED_EDGE('',*,*,#9578,.T.);
#12324=ORIENTED_EDGE('',*,*,#9461,.F.);
#12325=ORIENTED_EDGE('',*,*,#9435,.F.);
#12326=ORIENTED_EDGE('',*,*,#9429,.F.);
#12327=ORIENTED_EDGE('',*,*,#9432,.F.);
#12328=ORIENTED_EDGE('',*,*,#9438,.F.);
#12329=ORIENTED_EDGE('',*,*,#9579,.F.);
#12330=ORIENTED_EDGE('',*,*,#9580,.F.);
#12331=ORIENTED_EDGE('',*,*,#9581,.F.);
#12332=ORIENTED_EDGE('',*,*,#9582,.F.);
#12333=ORIENTED_EDGE('',*,*,#9583,.F.);
#12334=ORIENTED_EDGE('',*,*,#9584,.F.);
#12335=ORIENTED_EDGE('',*,*,#9585,.F.);
#12336=ORIENTED_EDGE('',*,*,#9586,.F.);
#12337=ORIENTED_EDGE('',*,*,#9440,.T.);
#12338=ORIENTED_EDGE('',*,*,#9437,.T.);
#12339=ORIENTED_EDGE('',*,*,#9434,.T.);
#12340=ORIENTED_EDGE('',*,*,#9431,.T.);
#12341=ORIENTED_EDGE('',*,*,#9458,.F.);
#12342=ORIENTED_EDGE('',*,*,#9579,.T.);
#12343=ORIENTED_EDGE('',*,*,#9587,.F.);
#12344=ORIENTED_EDGE('',*,*,#9571,.F.);
#12345=ORIENTED_EDGE('',*,*,#9588,.T.);
#12346=ORIENTED_EDGE('',*,*,#9586,.T.);
#12347=ORIENTED_EDGE('',*,*,#9589,.F.);
#12348=ORIENTED_EDGE('',*,*,#9572,.F.);
#12349=ORIENTED_EDGE('',*,*,#9587,.T.);
#12350=ORIENTED_EDGE('',*,*,#9585,.T.);
#12351=ORIENTED_EDGE('',*,*,#9590,.F.);
#12352=ORIENTED_EDGE('',*,*,#9573,.F.);
#12353=ORIENTED_EDGE('',*,*,#9589,.T.);
#12354=ORIENTED_EDGE('',*,*,#9584,.T.);
#12355=ORIENTED_EDGE('',*,*,#9591,.F.);
#12356=ORIENTED_EDGE('',*,*,#9574,.F.);
#12357=ORIENTED_EDGE('',*,*,#9590,.T.);
#12358=ORIENTED_EDGE('',*,*,#9583,.T.);
#12359=ORIENTED_EDGE('',*,*,#9592,.F.);
#12360=ORIENTED_EDGE('',*,*,#9575,.F.);
#12361=ORIENTED_EDGE('',*,*,#9591,.T.);
#12362=ORIENTED_EDGE('',*,*,#9582,.T.);
#12363=ORIENTED_EDGE('',*,*,#9593,.F.);
#12364=ORIENTED_EDGE('',*,*,#9576,.F.);
#12365=ORIENTED_EDGE('',*,*,#9592,.T.);
#12366=ORIENTED_EDGE('',*,*,#9581,.T.);
#12367=ORIENTED_EDGE('',*,*,#9594,.F.);
#12368=ORIENTED_EDGE('',*,*,#9577,.F.);
#12369=ORIENTED_EDGE('',*,*,#9593,.T.);
#12370=ORIENTED_EDGE('',*,*,#9580,.T.);
#12371=ORIENTED_EDGE('',*,*,#9588,.F.);
#12372=ORIENTED_EDGE('',*,*,#9578,.F.);
#12373=ORIENTED_EDGE('',*,*,#9594,.T.);
#12374=ORIENTED_EDGE('',*,*,#9408,.T.);
#12375=ORIENTED_EDGE('',*,*,#9466,.F.);
#12376=ORIENTED_EDGE('',*,*,#9418,.F.);
#12377=ORIENTED_EDGE('',*,*,#9544,.T.);
#12378=ORIENTED_EDGE('',*,*,#9595,.T.);
#12379=ORIENTED_EDGE('',*,*,#9542,.F.);
#12380=ORIENTED_EDGE('',*,*,#9420,.T.);
#12381=ORIENTED_EDGE('',*,*,#9596,.F.);
#12382=ORIENTED_EDGE('',*,*,#9596,.T.);
#12383=ORIENTED_EDGE('',*,*,#9419,.T.);
#12384=ORIENTED_EDGE('',*,*,#9595,.F.);
#12385=ORIENTED_EDGE('',*,*,#9543,.T.);
#12386=ORIENTED_EDGE('',*,*,#9422,.F.);
#12387=ORIENTED_EDGE('',*,*,#9541,.T.);
#12388=ORIENTED_EDGE('',*,*,#9597,.T.);
#12389=ORIENTED_EDGE('',*,*,#9539,.F.);
#12390=ORIENTED_EDGE('',*,*,#9424,.T.);
#12391=ORIENTED_EDGE('',*,*,#9598,.F.);
#12392=ORIENTED_EDGE('',*,*,#9598,.T.);
#12393=ORIENTED_EDGE('',*,*,#9423,.T.);
#12394=ORIENTED_EDGE('',*,*,#9597,.F.);
#12395=ORIENTED_EDGE('',*,*,#9540,.T.);
#12396=ORIENTED_EDGE('',*,*,#9426,.F.);
#12397=ORIENTED_EDGE('',*,*,#9538,.T.);
#12398=ORIENTED_EDGE('',*,*,#9599,.T.);
#12399=ORIENTED_EDGE('',*,*,#9536,.F.);
#12400=ORIENTED_EDGE('',*,*,#9428,.T.);
#12401=ORIENTED_EDGE('',*,*,#9600,.F.);
#12402=ORIENTED_EDGE('',*,*,#9600,.T.);
#12403=ORIENTED_EDGE('',*,*,#9427,.T.);
#12404=ORIENTED_EDGE('',*,*,#9599,.F.);
#12405=ORIENTED_EDGE('',*,*,#9537,.T.);
#12406=ORIENTED_EDGE('',*,*,#9391,.F.);
#12407=ORIENTED_EDGE('',*,*,#9535,.T.);
#12408=ORIENTED_EDGE('',*,*,#9601,.T.);
#12409=ORIENTED_EDGE('',*,*,#9533,.F.);
#12410=ORIENTED_EDGE('',*,*,#9393,.T.);
#12411=ORIENTED_EDGE('',*,*,#9602,.F.);
#12412=ORIENTED_EDGE('',*,*,#9602,.T.);
#12413=ORIENTED_EDGE('',*,*,#9392,.T.);
#12414=ORIENTED_EDGE('',*,*,#9601,.F.);
#12415=ORIENTED_EDGE('',*,*,#9534,.T.);
#12416=ORIENTED_EDGE('',*,*,#9395,.F.);
#12417=ORIENTED_EDGE('',*,*,#9532,.T.);
#12418=ORIENTED_EDGE('',*,*,#9603,.T.);
#12419=ORIENTED_EDGE('',*,*,#9530,.F.);
#12420=ORIENTED_EDGE('',*,*,#9397,.T.);
#12421=ORIENTED_EDGE('',*,*,#9604,.F.);
#12422=ORIENTED_EDGE('',*,*,#9604,.T.);
#12423=ORIENTED_EDGE('',*,*,#9396,.T.);
#12424=ORIENTED_EDGE('',*,*,#9603,.F.);
#12425=ORIENTED_EDGE('',*,*,#9531,.T.);
#12426=ORIENTED_EDGE('',*,*,#9399,.F.);
#12427=ORIENTED_EDGE('',*,*,#9529,.T.);
#12428=ORIENTED_EDGE('',*,*,#9605,.T.);
#12429=ORIENTED_EDGE('',*,*,#9527,.F.);
#12430=ORIENTED_EDGE('',*,*,#9401,.T.);
#12431=ORIENTED_EDGE('',*,*,#9606,.F.);
#12432=ORIENTED_EDGE('',*,*,#9606,.T.);
#12433=ORIENTED_EDGE('',*,*,#9400,.T.);
#12434=ORIENTED_EDGE('',*,*,#9605,.F.);
#12435=ORIENTED_EDGE('',*,*,#9528,.T.);
#12436=ORIENTED_EDGE('',*,*,#9403,.F.);
#12437=ORIENTED_EDGE('',*,*,#9526,.T.);
#12438=ORIENTED_EDGE('',*,*,#9607,.T.);
#12439=ORIENTED_EDGE('',*,*,#9524,.F.);
#12440=ORIENTED_EDGE('',*,*,#9405,.T.);
#12441=ORIENTED_EDGE('',*,*,#9608,.F.);
#12442=ORIENTED_EDGE('',*,*,#9608,.T.);
#12443=ORIENTED_EDGE('',*,*,#9404,.T.);
#12444=ORIENTED_EDGE('',*,*,#9607,.F.);
#12445=ORIENTED_EDGE('',*,*,#9525,.T.);
#12446=ORIENTED_EDGE('',*,*,#9410,.F.);
#12447=ORIENTED_EDGE('',*,*,#9523,.T.);
#12448=ORIENTED_EDGE('',*,*,#9609,.T.);
#12449=ORIENTED_EDGE('',*,*,#9521,.F.);
#12450=ORIENTED_EDGE('',*,*,#9412,.T.);
#12451=ORIENTED_EDGE('',*,*,#9610,.F.);
#12452=ORIENTED_EDGE('',*,*,#9610,.T.);
#12453=ORIENTED_EDGE('',*,*,#9411,.T.);
#12454=ORIENTED_EDGE('',*,*,#9609,.F.);
#12455=ORIENTED_EDGE('',*,*,#9522,.T.);
#12456=ORIENTED_EDGE('',*,*,#9414,.F.);
#12457=ORIENTED_EDGE('',*,*,#9520,.T.);
#12458=ORIENTED_EDGE('',*,*,#9611,.T.);
#12459=ORIENTED_EDGE('',*,*,#9545,.F.);
#12460=ORIENTED_EDGE('',*,*,#9416,.T.);
#12461=ORIENTED_EDGE('',*,*,#9612,.F.);
#12462=ORIENTED_EDGE('',*,*,#9612,.T.);
#12463=ORIENTED_EDGE('',*,*,#9415,.T.);
#12464=ORIENTED_EDGE('',*,*,#9611,.F.);
#12465=ORIENTED_EDGE('',*,*,#9546,.T.);
#12466=ORIENTED_EDGE('',*,*,#9613,.T.);
#12467=ORIENTED_EDGE('',*,*,#9614,.T.);
#12468=ORIENTED_EDGE('',*,*,#9615,.F.);
#12469=ORIENTED_EDGE('',*,*,#9616,.F.);
#12470=ORIENTED_EDGE('',*,*,#9617,.T.);
#12471=ORIENTED_EDGE('',*,*,#9616,.T.);
#12472=ORIENTED_EDGE('',*,*,#9618,.F.);
#12473=ORIENTED_EDGE('',*,*,#9614,.F.);
#12474=ORIENTED_EDGE('',*,*,#9619,.F.);
#12475=ORIENTED_EDGE('',*,*,#9620,.T.);
#12476=ORIENTED_EDGE('',*,*,#9621,.F.);
#12477=ORIENTED_EDGE('',*,*,#9622,.F.);
#12478=ORIENTED_EDGE('',*,*,#9623,.F.);
#12479=ORIENTED_EDGE('',*,*,#9624,.F.);
#12480=ORIENTED_EDGE('',*,*,#9625,.F.);
#12481=ORIENTED_EDGE('',*,*,#9626,.F.);
#12482=ORIENTED_EDGE('',*,*,#9627,.F.);
#12483=ORIENTED_EDGE('',*,*,#9628,.F.);
#12484=ORIENTED_EDGE('',*,*,#9620,.F.);
#12485=ORIENTED_EDGE('',*,*,#9629,.F.);
#12486=ORIENTED_EDGE('',*,*,#9630,.F.);
#12487=ORIENTED_EDGE('',*,*,#9631,.T.);
#12488=ORIENTED_EDGE('',*,*,#9632,.F.);
#12489=ORIENTED_EDGE('',*,*,#9633,.F.);
#12490=ORIENTED_EDGE('',*,*,#9631,.F.);
#12491=ORIENTED_EDGE('',*,*,#9618,.T.);
#12492=ORIENTED_EDGE('',*,*,#9615,.T.);
#12493=ORIENTED_EDGE('',*,*,#9634,.F.);
#12494=ORIENTED_EDGE('',*,*,#9629,.T.);
#12495=ORIENTED_EDGE('',*,*,#9635,.F.);
#12496=ORIENTED_EDGE('',*,*,#9636,.F.);
#12497=ORIENTED_EDGE('',*,*,#9619,.T.);
#12498=ORIENTED_EDGE('',*,*,#9635,.T.);
#12499=ORIENTED_EDGE('',*,*,#9637,.F.);
#12500=ORIENTED_EDGE('',*,*,#9638,.F.);
#12501=ORIENTED_EDGE('',*,*,#9639,.T.);
#12502=ORIENTED_EDGE('',*,*,#9636,.T.);
#12503=ORIENTED_EDGE('',*,*,#9639,.F.);
#12504=ORIENTED_EDGE('',*,*,#9640,.F.);
#12505=ORIENTED_EDGE('',*,*,#9637,.T.);
#12506=ORIENTED_EDGE('',*,*,#9638,.T.);
#12507=ORIENTED_EDGE('',*,*,#9640,.T.);
#12508=ORIENTED_EDGE('',*,*,#9617,.F.);
#12509=ORIENTED_EDGE('',*,*,#9613,.F.);
#12510=ORIENTED_EDGE('',*,*,#9622,.T.);
#12511=ORIENTED_EDGE('',*,*,#9641,.T.);
#12512=ORIENTED_EDGE('',*,*,#9621,.T.);
#12513=ORIENTED_EDGE('',*,*,#9642,.T.);
#12514=ORIENTED_EDGE('',*,*,#9628,.T.);
#12515=ORIENTED_EDGE('',*,*,#9643,.T.);
#12516=ORIENTED_EDGE('',*,*,#9627,.T.);
#12517=ORIENTED_EDGE('',*,*,#9644,.T.);
#12518=ORIENTED_EDGE('',*,*,#9626,.T.);
#12519=ORIENTED_EDGE('',*,*,#9645,.T.);
#12520=ORIENTED_EDGE('',*,*,#9625,.T.);
#12521=ORIENTED_EDGE('',*,*,#9646,.T.);
#12522=ORIENTED_EDGE('',*,*,#9624,.T.);
#12523=ORIENTED_EDGE('',*,*,#9647,.T.);
#12524=ORIENTED_EDGE('',*,*,#9623,.T.);
#12525=ORIENTED_EDGE('',*,*,#9648,.T.);
#12526=ORIENTED_EDGE('',*,*,#9649,.T.);
#12527=ORIENTED_EDGE('',*,*,#9650,.T.);
#12528=ORIENTED_EDGE('',*,*,#9651,.F.);
#12529=ORIENTED_EDGE('',*,*,#9652,.F.);
#12530=ORIENTED_EDGE('',*,*,#9653,.T.);
#12531=ORIENTED_EDGE('',*,*,#9652,.T.);
#12532=ORIENTED_EDGE('',*,*,#9654,.F.);
#12533=ORIENTED_EDGE('',*,*,#9650,.F.);
#12534=ORIENTED_EDGE('',*,*,#9655,.F.);
#12535=ORIENTED_EDGE('',*,*,#9656,.T.);
#12536=ORIENTED_EDGE('',*,*,#9657,.F.);
#12537=ORIENTED_EDGE('',*,*,#9658,.F.);
#12538=ORIENTED_EDGE('',*,*,#9659,.F.);
#12539=ORIENTED_EDGE('',*,*,#9660,.F.);
#12540=ORIENTED_EDGE('',*,*,#9661,.F.);
#12541=ORIENTED_EDGE('',*,*,#9662,.F.);
#12542=ORIENTED_EDGE('',*,*,#9663,.F.);
#12543=ORIENTED_EDGE('',*,*,#9664,.F.);
#12544=ORIENTED_EDGE('',*,*,#9656,.F.);
#12545=ORIENTED_EDGE('',*,*,#9665,.F.);
#12546=ORIENTED_EDGE('',*,*,#9666,.F.);
#12547=ORIENTED_EDGE('',*,*,#9667,.T.);
#12548=ORIENTED_EDGE('',*,*,#9668,.F.);
#12549=ORIENTED_EDGE('',*,*,#9669,.F.);
#12550=ORIENTED_EDGE('',*,*,#9667,.F.);
#12551=ORIENTED_EDGE('',*,*,#9670,.F.);
#12552=ORIENTED_EDGE('',*,*,#9654,.T.);
#12553=ORIENTED_EDGE('',*,*,#9651,.T.);
#12554=ORIENTED_EDGE('',*,*,#9671,.F.);
#12555=ORIENTED_EDGE('',*,*,#9665,.T.);
#12556=ORIENTED_EDGE('',*,*,#9672,.F.);
#12557=ORIENTED_EDGE('',*,*,#9673,.F.);
#12558=ORIENTED_EDGE('',*,*,#9674,.F.);
#12559=ORIENTED_EDGE('',*,*,#9655,.T.);
#12560=ORIENTED_EDGE('',*,*,#9673,.T.);
#12561=ORIENTED_EDGE('',*,*,#9675,.F.);
#12562=ORIENTED_EDGE('',*,*,#9676,.F.);
#12563=ORIENTED_EDGE('',*,*,#9677,.T.);
#12564=ORIENTED_EDGE('',*,*,#9674,.T.);
#12565=ORIENTED_EDGE('',*,*,#9677,.F.);
#12566=ORIENTED_EDGE('',*,*,#9678,.F.);
#12567=ORIENTED_EDGE('',*,*,#9675,.T.);
#12568=ORIENTED_EDGE('',*,*,#9676,.T.);
#12569=ORIENTED_EDGE('',*,*,#9678,.T.);
#12570=ORIENTED_EDGE('',*,*,#9653,.F.);
#12571=ORIENTED_EDGE('',*,*,#9649,.F.);
#12572=ORIENTED_EDGE('',*,*,#9661,.T.);
#12573=ORIENTED_EDGE('',*,*,#9679,.F.);
#12574=ORIENTED_EDGE('',*,*,#9660,.T.);
#12575=ORIENTED_EDGE('',*,*,#9680,.F.);
#12576=ORIENTED_EDGE('',*,*,#9659,.T.);
#12577=ORIENTED_EDGE('',*,*,#9681,.F.);
#12578=ORIENTED_EDGE('',*,*,#9658,.T.);
#12579=ORIENTED_EDGE('',*,*,#9682,.F.);
#12580=ORIENTED_EDGE('',*,*,#9657,.T.);
#12581=ORIENTED_EDGE('',*,*,#9683,.F.);
#12582=ORIENTED_EDGE('',*,*,#9664,.T.);
#12583=ORIENTED_EDGE('',*,*,#9684,.F.);
#12584=ORIENTED_EDGE('',*,*,#9663,.T.);
#12585=ORIENTED_EDGE('',*,*,#9685,.F.);
#12586=ORIENTED_EDGE('',*,*,#9662,.T.);
#12587=ORIENTED_EDGE('',*,*,#9686,.F.);
#12588=ORIENTED_EDGE('',*,*,#9646,.F.);
#12589=ORIENTED_EDGE('',*,*,#9687,.T.);
#12590=ORIENTED_EDGE('',*,*,#9688,.T.);
#12591=ORIENTED_EDGE('',*,*,#9689,.F.);
#12592=ORIENTED_EDGE('',*,*,#9643,.F.);
#12593=ORIENTED_EDGE('',*,*,#9644,.F.);
#12594=ORIENTED_EDGE('',*,*,#9645,.F.);
#12595=ORIENTED_EDGE('',*,*,#9690,.F.);
#12596=ORIENTED_EDGE('',*,*,#9691,.F.);
#12597=ORIENTED_EDGE('',*,*,#9692,.F.);
#12598=ORIENTED_EDGE('',*,*,#9693,.F.);
#12599=ORIENTED_EDGE('',*,*,#9694,.F.);
#12600=ORIENTED_EDGE('',*,*,#9695,.F.);
#12601=ORIENTED_EDGE('',*,*,#9696,.F.);
#12602=ORIENTED_EDGE('',*,*,#9697,.F.);
#12603=ORIENTED_EDGE('',*,*,#9680,.T.);
#12604=ORIENTED_EDGE('',*,*,#9681,.T.);
#12605=ORIENTED_EDGE('',*,*,#9682,.T.);
#12606=ORIENTED_EDGE('',*,*,#9683,.T.);
#12607=ORIENTED_EDGE('',*,*,#9698,.T.);
#12608=ORIENTED_EDGE('',*,*,#9699,.F.);
#12609=ORIENTED_EDGE('',*,*,#9700,.F.);
#12610=ORIENTED_EDGE('',*,*,#9701,.F.);
#12611=ORIENTED_EDGE('',*,*,#9702,.T.);
#12612=ORIENTED_EDGE('',*,*,#9703,.T.);
#12613=ORIENTED_EDGE('',*,*,#9704,.F.);
#12614=ORIENTED_EDGE('',*,*,#9705,.T.);
#12615=ORIENTED_EDGE('',*,*,#9706,.T.);
#12616=ORIENTED_EDGE('',*,*,#9707,.T.);
#12617=ORIENTED_EDGE('',*,*,#9708,.T.);
#12618=ORIENTED_EDGE('',*,*,#9709,.T.);
#12619=ORIENTED_EDGE('',*,*,#9710,.T.);
#12620=ORIENTED_EDGE('',*,*,#9711,.F.);
#12621=ORIENTED_EDGE('',*,*,#9712,.F.);
#12622=ORIENTED_EDGE('',*,*,#9713,.T.);
#12623=ORIENTED_EDGE('',*,*,#9714,.T.);
#12624=ORIENTED_EDGE('',*,*,#9672,.T.);
#12625=ORIENTED_EDGE('',*,*,#9668,.T.);
#12626=ORIENTED_EDGE('',*,*,#9669,.T.);
#12627=ORIENTED_EDGE('',*,*,#9715,.T.);
#12628=ORIENTED_EDGE('',*,*,#9716,.F.);
#12629=ORIENTED_EDGE('',*,*,#9715,.F.);
#12630=ORIENTED_EDGE('',*,*,#9670,.T.);
#12631=ORIENTED_EDGE('',*,*,#9666,.T.);
#12632=ORIENTED_EDGE('',*,*,#9671,.T.);
#12633=ORIENTED_EDGE('',*,*,#9714,.F.);
#12634=ORIENTED_EDGE('',*,*,#9632,.T.);
#12635=ORIENTED_EDGE('',*,*,#9633,.T.);
#12636=ORIENTED_EDGE('',*,*,#9630,.T.);
#12637=ORIENTED_EDGE('',*,*,#9634,.T.);
#12638=ORIENTED_EDGE('',*,*,#9717,.T.);
#12639=ORIENTED_EDGE('',*,*,#9718,.T.);
#12640=ORIENTED_EDGE('',*,*,#9699,.T.);
#12641=ORIENTED_EDGE('',*,*,#9719,.T.);
#12642=ORIENTED_EDGE('',*,*,#9720,.T.);
#12643=ORIENTED_EDGE('',*,*,#9721,.F.);
#12644=ORIENTED_EDGE('',*,*,#9720,.F.);
#12645=ORIENTED_EDGE('',*,*,#9722,.T.);
#12646=ORIENTED_EDGE('',*,*,#9718,.F.);
#12647=ORIENTED_EDGE('',*,*,#9688,.F.);
#12648=ORIENTED_EDGE('',*,*,#9723,.F.);
#12649=ORIENTED_EDGE('',*,*,#9724,.T.);
#12650=ORIENTED_EDGE('',*,*,#9693,.T.);
#12651=ORIENTED_EDGE('',*,*,#9725,.F.);
#12652=ORIENTED_EDGE('',*,*,#9726,.F.);
#12653=ORIENTED_EDGE('',*,*,#9727,.T.);
#12654=ORIENTED_EDGE('',*,*,#9728,.T.);
#12655=ORIENTED_EDGE('',*,*,#9704,.T.);
#12656=ORIENTED_EDGE('',*,*,#9729,.F.);
#12657=ORIENTED_EDGE('',*,*,#9730,.T.);
#12658=ORIENTED_EDGE('',*,*,#9731,.T.);
#12659=ORIENTED_EDGE('',*,*,#9732,.F.);
#12660=ORIENTED_EDGE('',*,*,#9702,.F.);
#12661=ORIENTED_EDGE('',*,*,#9695,.T.);
#12662=ORIENTED_EDGE('',*,*,#9733,.T.);
#12663=ORIENTED_EDGE('',*,*,#9734,.T.);
#12664=ORIENTED_EDGE('',*,*,#9735,.F.);
#12665=ORIENTED_EDGE('',*,*,#9703,.F.);
#12666=ORIENTED_EDGE('',*,*,#9732,.T.);
#12667=ORIENTED_EDGE('',*,*,#9736,.T.);
#12668=ORIENTED_EDGE('',*,*,#9737,.T.);
#12669=ORIENTED_EDGE('',*,*,#9738,.T.);
#12670=ORIENTED_EDGE('',*,*,#9739,.F.);
#12671=ORIENTED_EDGE('',*,*,#9696,.T.);
#12672=ORIENTED_EDGE('',*,*,#9735,.T.);
#12673=ORIENTED_EDGE('',*,*,#9740,.F.);
#12674=ORIENTED_EDGE('',*,*,#9725,.T.);
#12675=ORIENTED_EDGE('',*,*,#9692,.T.);
#12676=ORIENTED_EDGE('',*,*,#9741,.T.);
#12677=ORIENTED_EDGE('',*,*,#9742,.T.);
#12678=ORIENTED_EDGE('',*,*,#9743,.F.);
#12679=ORIENTED_EDGE('',*,*,#9744,.T.);
#12680=ORIENTED_EDGE('',*,*,#9729,.T.);
#12681=ORIENTED_EDGE('',*,*,#9745,.F.);
#12682=ORIENTED_EDGE('',*,*,#9746,.F.);
#12683=ORIENTED_EDGE('',*,*,#9747,.F.);
#12684=ORIENTED_EDGE('',*,*,#9748,.T.);
#12685=ORIENTED_EDGE('',*,*,#9749,.F.);
#12686=ORIENTED_EDGE('',*,*,#9750,.F.);
#12687=ORIENTED_EDGE('',*,*,#9709,.F.);
#12688=ORIENTED_EDGE('',*,*,#9751,.T.);
#12689=ORIENTED_EDGE('',*,*,#9752,.F.);
#12690=ORIENTED_EDGE('',*,*,#9753,.F.);
#12691=ORIENTED_EDGE('',*,*,#9754,.F.);
#12692=ORIENTED_EDGE('',*,*,#9755,.T.);
#12693=ORIENTED_EDGE('',*,*,#9756,.F.);
#12694=ORIENTED_EDGE('',*,*,#9757,.F.);
#12695=ORIENTED_EDGE('',*,*,#9758,.F.);
#12696=ORIENTED_EDGE('',*,*,#9759,.T.);
#12697=ORIENTED_EDGE('',*,*,#9760,.F.);
#12698=ORIENTED_EDGE('',*,*,#9761,.F.);
#12699=ORIENTED_EDGE('',*,*,#9762,.F.);
#12700=ORIENTED_EDGE('',*,*,#9763,.T.);
#12701=ORIENTED_EDGE('',*,*,#9764,.F.);
#12702=ORIENTED_EDGE('',*,*,#9765,.F.);
#12703=ORIENTED_EDGE('',*,*,#9766,.T.);
#12704=ORIENTED_EDGE('',*,*,#9767,.F.);
#12705=ORIENTED_EDGE('',*,*,#9768,.T.);
#12706=ORIENTED_EDGE('',*,*,#9769,.T.);
#12707=ORIENTED_EDGE('',*,*,#9770,.F.);
#12708=ORIENTED_EDGE('',*,*,#9771,.F.);
#12709=ORIENTED_EDGE('',*,*,#9772,.T.);
#12710=ORIENTED_EDGE('',*,*,#9773,.F.);
#12711=ORIENTED_EDGE('',*,*,#9774,.T.);
#12712=ORIENTED_EDGE('',*,*,#9775,.F.);
#12713=ORIENTED_EDGE('',*,*,#9776,.F.);
#12714=ORIENTED_EDGE('',*,*,#9777,.F.);
#12715=ORIENTED_EDGE('',*,*,#9778,.T.);
#12716=ORIENTED_EDGE('',*,*,#9779,.F.);
#12717=ORIENTED_EDGE('',*,*,#9780,.F.);
#12718=ORIENTED_EDGE('',*,*,#9781,.F.);
#12719=ORIENTED_EDGE('',*,*,#9782,.T.);
#12720=ORIENTED_EDGE('',*,*,#9747,.T.);
#12721=ORIENTED_EDGE('',*,*,#9783,.T.);
#12722=ORIENTED_EDGE('',*,*,#9784,.F.);
#12723=ORIENTED_EDGE('',*,*,#9785,.F.);
#12724=ORIENTED_EDGE('',*,*,#9754,.T.);
#12725=ORIENTED_EDGE('',*,*,#9786,.T.);
#12726=ORIENTED_EDGE('',*,*,#9787,.F.);
#12727=ORIENTED_EDGE('',*,*,#9788,.F.);
#12728=ORIENTED_EDGE('',*,*,#9758,.T.);
#12729=ORIENTED_EDGE('',*,*,#9789,.T.);
#12730=ORIENTED_EDGE('',*,*,#9790,.F.);
#12731=ORIENTED_EDGE('',*,*,#9791,.F.);
#12732=ORIENTED_EDGE('',*,*,#9762,.T.);
#12733=ORIENTED_EDGE('',*,*,#9792,.T.);
#12734=ORIENTED_EDGE('',*,*,#9793,.F.);
#12735=ORIENTED_EDGE('',*,*,#9794,.F.);
#12736=ORIENTED_EDGE('',*,*,#9767,.T.);
#12737=ORIENTED_EDGE('',*,*,#9795,.T.);
#12738=ORIENTED_EDGE('',*,*,#9796,.F.);
#12739=ORIENTED_EDGE('',*,*,#9797,.T.);
#12740=ORIENTED_EDGE('',*,*,#9798,.F.);
#12741=ORIENTED_EDGE('',*,*,#9781,.T.);
#12742=ORIENTED_EDGE('',*,*,#9799,.T.);
#12743=ORIENTED_EDGE('',*,*,#9800,.F.);
#12744=ORIENTED_EDGE('',*,*,#9773,.T.);
#12745=ORIENTED_EDGE('',*,*,#9801,.T.);
#12746=ORIENTED_EDGE('',*,*,#9802,.F.);
#12747=ORIENTED_EDGE('',*,*,#9803,.F.);
#12748=ORIENTED_EDGE('',*,*,#9777,.T.);
#12749=ORIENTED_EDGE('',*,*,#9804,.T.);
#12750=ORIENTED_EDGE('',*,*,#9805,.F.);
#12751=ORIENTED_EDGE('',*,*,#9806,.F.);
#12752=ORIENTED_EDGE('',*,*,#9716,.T.);
#12753=ORIENTED_EDGE('',*,*,#9717,.F.);
#12754=ORIENTED_EDGE('',*,*,#9713,.F.);
#12755=ORIENTED_EDGE('',*,*,#9721,.T.);
#12756=ORIENTED_EDGE('',*,*,#9737,.F.);
#12757=ORIENTED_EDGE('',*,*,#9807,.T.);
#12758=ORIENTED_EDGE('',*,*,#9808,.T.);
#12759=ORIENTED_EDGE('',*,*,#9809,.F.);
#12760=ORIENTED_EDGE('',*,*,#9810,.T.);
#12761=ORIENTED_EDGE('',*,*,#9811,.F.);
#12762=ORIENTED_EDGE('',*,*,#9738,.F.);
#12763=ORIENTED_EDGE('',*,*,#9809,.T.);
#12764=ORIENTED_EDGE('',*,*,#9812,.F.);
#12765=ORIENTED_EDGE('',*,*,#9697,.T.);
#12766=ORIENTED_EDGE('',*,*,#9739,.T.);
#12767=ORIENTED_EDGE('',*,*,#9811,.T.);
#12768=ORIENTED_EDGE('',*,*,#9741,.F.);
#12769=ORIENTED_EDGE('',*,*,#9691,.T.);
#12770=ORIENTED_EDGE('',*,*,#9813,.T.);
#12771=ORIENTED_EDGE('',*,*,#9814,.F.);
#12772=ORIENTED_EDGE('',*,*,#9815,.T.);
#12773=ORIENTED_EDGE('',*,*,#9816,.F.);
#12774=ORIENTED_EDGE('',*,*,#9742,.F.);
#12775=ORIENTED_EDGE('',*,*,#9814,.T.);
#12776=ORIENTED_EDGE('',*,*,#9817,.F.);
#12777=ORIENTED_EDGE('',*,*,#9818,.T.);
#12778=ORIENTED_EDGE('',*,*,#9743,.T.);
#12779=ORIENTED_EDGE('',*,*,#9816,.T.);
#12780=ORIENTED_EDGE('',*,*,#9730,.F.);
#12781=ORIENTED_EDGE('',*,*,#9701,.T.);
#12782=ORIENTED_EDGE('',*,*,#9728,.F.);
#12783=ORIENTED_EDGE('',*,*,#9819,.T.);
#12784=ORIENTED_EDGE('',*,*,#9817,.T.);
#12785=ORIENTED_EDGE('',*,*,#9815,.F.);
#12786=ORIENTED_EDGE('',*,*,#9813,.F.);
#12787=ORIENTED_EDGE('',*,*,#9690,.T.);
#12788=ORIENTED_EDGE('',*,*,#9724,.F.);
#12789=ORIENTED_EDGE('',*,*,#9820,.T.);
#12790=ORIENTED_EDGE('',*,*,#9733,.F.);
#12791=ORIENTED_EDGE('',*,*,#9694,.T.);
#12792=ORIENTED_EDGE('',*,*,#9812,.T.);
#12793=ORIENTED_EDGE('',*,*,#9810,.F.);
#12794=ORIENTED_EDGE('',*,*,#9808,.F.);
#12795=ORIENTED_EDGE('',*,*,#9821,.T.);
#12796=ORIENTED_EDGE('',*,*,#9705,.F.);
#12797=ORIENTED_EDGE('',*,*,#9822,.T.);
#12798=ORIENTED_EDGE('',*,*,#9823,.T.);
#12799=ORIENTED_EDGE('',*,*,#9824,.T.);
#12800=ORIENTED_EDGE('',*,*,#9784,.T.);
#12801=ORIENTED_EDGE('',*,*,#9825,.F.);
#12802=ORIENTED_EDGE('',*,*,#9826,.T.);
#12803=ORIENTED_EDGE('',*,*,#9827,.T.);
#12804=ORIENTED_EDGE('',*,*,#9800,.T.);
#12805=ORIENTED_EDGE('',*,*,#9828,.F.);
#12806=ORIENTED_EDGE('',*,*,#9829,.T.);
#12807=ORIENTED_EDGE('',*,*,#9830,.T.);
#12808=ORIENTED_EDGE('',*,*,#9805,.T.);
#12809=ORIENTED_EDGE('',*,*,#9831,.F.);
#12810=ORIENTED_EDGE('',*,*,#9832,.T.);
#12811=ORIENTED_EDGE('',*,*,#9833,.T.);
#12812=ORIENTED_EDGE('',*,*,#9802,.T.);
#12813=ORIENTED_EDGE('',*,*,#9834,.F.);
#12814=ORIENTED_EDGE('',*,*,#9835,.F.);
#12815=ORIENTED_EDGE('',*,*,#9836,.T.);
#12816=ORIENTED_EDGE('',*,*,#9837,.T.);
#12817=ORIENTED_EDGE('',*,*,#9838,.F.);
#12818=ORIENTED_EDGE('',*,*,#9796,.T.);
#12819=ORIENTED_EDGE('',*,*,#9839,.F.);
#12820=ORIENTED_EDGE('',*,*,#9840,.F.);
#12821=ORIENTED_EDGE('',*,*,#9841,.T.);
#12822=ORIENTED_EDGE('',*,*,#9842,.T.);
#12823=ORIENTED_EDGE('',*,*,#9793,.T.);
#12824=ORIENTED_EDGE('',*,*,#9843,.F.);
#12825=ORIENTED_EDGE('',*,*,#9844,.T.);
#12826=ORIENTED_EDGE('',*,*,#9845,.T.);
#12827=ORIENTED_EDGE('',*,*,#9790,.T.);
#12828=ORIENTED_EDGE('',*,*,#9846,.F.);
#12829=ORIENTED_EDGE('',*,*,#9847,.T.);
#12830=ORIENTED_EDGE('',*,*,#9848,.T.);
#12831=ORIENTED_EDGE('',*,*,#9787,.T.);
#12832=ORIENTED_EDGE('',*,*,#9849,.F.);
#12833=ORIENTED_EDGE('',*,*,#9850,.T.);
#12834=ORIENTED_EDGE('',*,*,#9851,.T.);
#12835=ORIENTED_EDGE('',*,*,#9711,.T.);
#12836=ORIENTED_EDGE('',*,*,#9852,.F.);
#12837=ORIENTED_EDGE('',*,*,#9853,.T.);
#12838=ORIENTED_EDGE('',*,*,#9854,.T.);
#12839=ORIENTED_EDGE('',*,*,#9855,.F.);
#12840=ORIENTED_EDGE('',*,*,#9707,.F.);
#12841=ORIENTED_EDGE('',*,*,#9856,.F.);
#12842=ORIENTED_EDGE('',*,*,#9857,.F.);
#12843=ORIENTED_EDGE('',*,*,#9740,.T.);
#12844=ORIENTED_EDGE('',*,*,#9734,.F.);
#12845=ORIENTED_EDGE('',*,*,#9820,.F.);
#12846=ORIENTED_EDGE('',*,*,#9726,.T.);
#12847=ORIENTED_EDGE('',*,*,#9858,.T.);
#12848=ORIENTED_EDGE('',*,*,#9829,.F.);
#12849=ORIENTED_EDGE('',*,*,#9859,.F.);
#12850=ORIENTED_EDGE('',*,*,#9779,.T.);
#12851=ORIENTED_EDGE('',*,*,#9799,.F.);
#12852=ORIENTED_EDGE('',*,*,#9780,.T.);
#12853=ORIENTED_EDGE('',*,*,#9859,.T.);
#12854=ORIENTED_EDGE('',*,*,#9828,.T.);
#12855=ORIENTED_EDGE('',*,*,#9778,.F.);
#12856=ORIENTED_EDGE('',*,*,#9806,.T.);
#12857=ORIENTED_EDGE('',*,*,#9830,.F.);
#12858=ORIENTED_EDGE('',*,*,#9858,.F.);
#12859=ORIENTED_EDGE('',*,*,#9860,.T.);
#12860=ORIENTED_EDGE('',*,*,#9832,.F.);
#12861=ORIENTED_EDGE('',*,*,#9861,.F.);
#12862=ORIENTED_EDGE('',*,*,#9775,.T.);
#12863=ORIENTED_EDGE('',*,*,#9804,.F.);
#12864=ORIENTED_EDGE('',*,*,#9776,.T.);
#12865=ORIENTED_EDGE('',*,*,#9861,.T.);
#12866=ORIENTED_EDGE('',*,*,#9831,.T.);
#12867=ORIENTED_EDGE('',*,*,#9774,.F.);
#12868=ORIENTED_EDGE('',*,*,#9803,.T.);
#12869=ORIENTED_EDGE('',*,*,#9833,.F.);
#12870=ORIENTED_EDGE('',*,*,#9860,.F.);
#12871=ORIENTED_EDGE('',*,*,#9797,.F.);
#12872=ORIENTED_EDGE('',*,*,#9838,.T.);
#12873=ORIENTED_EDGE('',*,*,#9862,.T.);
#12874=ORIENTED_EDGE('',*,*,#9768,.F.);
#12875=ORIENTED_EDGE('',*,*,#9801,.F.);
#12876=ORIENTED_EDGE('',*,*,#9772,.F.);
#12877=ORIENTED_EDGE('',*,*,#9863,.F.);
#12878=ORIENTED_EDGE('',*,*,#9834,.T.);
#12879=ORIENTED_EDGE('',*,*,#9864,.T.);
#12880=ORIENTED_EDGE('',*,*,#9836,.F.);
#12881=ORIENTED_EDGE('',*,*,#9865,.F.);
#12882=ORIENTED_EDGE('',*,*,#9770,.T.);
#12883=ORIENTED_EDGE('',*,*,#9863,.T.);
#12884=ORIENTED_EDGE('',*,*,#9771,.T.);
#12885=ORIENTED_EDGE('',*,*,#9865,.T.);
#12886=ORIENTED_EDGE('',*,*,#9835,.T.);
#12887=ORIENTED_EDGE('',*,*,#9862,.F.);
#12888=ORIENTED_EDGE('',*,*,#9837,.F.);
#12889=ORIENTED_EDGE('',*,*,#9864,.F.);
#12890=ORIENTED_EDGE('',*,*,#9769,.F.);
#12891=ORIENTED_EDGE('',*,*,#9795,.F.);
#12892=ORIENTED_EDGE('',*,*,#9766,.F.);
#12893=ORIENTED_EDGE('',*,*,#9866,.F.);
#12894=ORIENTED_EDGE('',*,*,#9839,.T.);
#12895=ORIENTED_EDGE('',*,*,#9867,.T.);
#12896=ORIENTED_EDGE('',*,*,#9841,.F.);
#12897=ORIENTED_EDGE('',*,*,#9868,.F.);
#12898=ORIENTED_EDGE('',*,*,#9764,.T.);
#12899=ORIENTED_EDGE('',*,*,#9866,.T.);
#12900=ORIENTED_EDGE('',*,*,#9765,.T.);
#12901=ORIENTED_EDGE('',*,*,#9868,.T.);
#12902=ORIENTED_EDGE('',*,*,#9840,.T.);
#12903=ORIENTED_EDGE('',*,*,#9763,.F.);
#12904=ORIENTED_EDGE('',*,*,#9794,.T.);
#12905=ORIENTED_EDGE('',*,*,#9842,.F.);
#12906=ORIENTED_EDGE('',*,*,#9867,.F.);
#12907=ORIENTED_EDGE('',*,*,#9869,.T.);
#12908=ORIENTED_EDGE('',*,*,#9844,.F.);
#12909=ORIENTED_EDGE('',*,*,#9870,.F.);
#12910=ORIENTED_EDGE('',*,*,#9760,.T.);
#12911=ORIENTED_EDGE('',*,*,#9792,.F.);
#12912=ORIENTED_EDGE('',*,*,#9761,.T.);
#12913=ORIENTED_EDGE('',*,*,#9870,.T.);
#12914=ORIENTED_EDGE('',*,*,#9843,.T.);
#12915=ORIENTED_EDGE('',*,*,#9759,.F.);
#12916=ORIENTED_EDGE('',*,*,#9791,.T.);
#12917=ORIENTED_EDGE('',*,*,#9845,.F.);
#12918=ORIENTED_EDGE('',*,*,#9869,.F.);
#12919=ORIENTED_EDGE('',*,*,#9871,.T.);
#12920=ORIENTED_EDGE('',*,*,#9847,.F.);
#12921=ORIENTED_EDGE('',*,*,#9872,.F.);
#12922=ORIENTED_EDGE('',*,*,#9756,.T.);
#12923=ORIENTED_EDGE('',*,*,#9789,.F.);
#12924=ORIENTED_EDGE('',*,*,#9757,.T.);
#12925=ORIENTED_EDGE('',*,*,#9872,.T.);
#12926=ORIENTED_EDGE('',*,*,#9846,.T.);
#12927=ORIENTED_EDGE('',*,*,#9755,.F.);
#12928=ORIENTED_EDGE('',*,*,#9788,.T.);
#12929=ORIENTED_EDGE('',*,*,#9848,.F.);
#12930=ORIENTED_EDGE('',*,*,#9871,.F.);
#12931=ORIENTED_EDGE('',*,*,#9873,.T.);
#12932=ORIENTED_EDGE('',*,*,#9850,.F.);
#12933=ORIENTED_EDGE('',*,*,#9874,.F.);
#12934=ORIENTED_EDGE('',*,*,#9752,.T.);
#12935=ORIENTED_EDGE('',*,*,#9786,.F.);
#12936=ORIENTED_EDGE('',*,*,#9753,.T.);
#12937=ORIENTED_EDGE('',*,*,#9874,.T.);
#12938=ORIENTED_EDGE('',*,*,#9849,.T.);
#12939=ORIENTED_EDGE('',*,*,#9751,.F.);
#12940=ORIENTED_EDGE('',*,*,#9712,.T.);
#12941=ORIENTED_EDGE('',*,*,#9851,.F.);
#12942=ORIENTED_EDGE('',*,*,#9873,.F.);
#12943=ORIENTED_EDGE('',*,*,#9875,.T.);
#12944=ORIENTED_EDGE('',*,*,#9853,.F.);
#12945=ORIENTED_EDGE('',*,*,#9876,.F.);
#12946=ORIENTED_EDGE('',*,*,#9749,.T.);
#12947=ORIENTED_EDGE('',*,*,#9710,.F.);
#12948=ORIENTED_EDGE('',*,*,#9750,.T.);
#12949=ORIENTED_EDGE('',*,*,#9876,.T.);
#12950=ORIENTED_EDGE('',*,*,#9852,.T.);
#12951=ORIENTED_EDGE('',*,*,#9748,.F.);
#12952=ORIENTED_EDGE('',*,*,#9785,.T.);
#12953=ORIENTED_EDGE('',*,*,#9854,.F.);
#12954=ORIENTED_EDGE('',*,*,#9875,.F.);
#12955=ORIENTED_EDGE('',*,*,#9877,.T.);
#12956=ORIENTED_EDGE('',*,*,#9826,.F.);
#12957=ORIENTED_EDGE('',*,*,#9878,.F.);
#12958=ORIENTED_EDGE('',*,*,#9745,.T.);
#12959=ORIENTED_EDGE('',*,*,#9783,.F.);
#12960=ORIENTED_EDGE('',*,*,#9746,.T.);
#12961=ORIENTED_EDGE('',*,*,#9878,.T.);
#12962=ORIENTED_EDGE('',*,*,#9825,.T.);
#12963=ORIENTED_EDGE('',*,*,#9782,.F.);
#12964=ORIENTED_EDGE('',*,*,#9798,.T.);
#12965=ORIENTED_EDGE('',*,*,#9827,.F.);
#12966=ORIENTED_EDGE('',*,*,#9877,.F.);
#12967=ORIENTED_EDGE('',*,*,#9698,.F.);
#12968=ORIENTED_EDGE('',*,*,#9684,.T.);
#12969=ORIENTED_EDGE('',*,*,#9685,.T.);
#12970=ORIENTED_EDGE('',*,*,#9686,.T.);
#12971=ORIENTED_EDGE('',*,*,#9679,.T.);
#12972=ORIENTED_EDGE('',*,*,#9700,.T.);
#12973=ORIENTED_EDGE('',*,*,#9722,.F.);
#12974=ORIENTED_EDGE('',*,*,#9719,.F.);
#12975=ORIENTED_EDGE('',*,*,#9736,.F.);
#12976=ORIENTED_EDGE('',*,*,#9731,.F.);
#12977=ORIENTED_EDGE('',*,*,#9821,.F.);
#12978=ORIENTED_EDGE('',*,*,#9807,.F.);
#12979=ORIENTED_EDGE('',*,*,#9744,.F.);
#12980=ORIENTED_EDGE('',*,*,#9818,.F.);
#12981=ORIENTED_EDGE('',*,*,#9819,.F.);
#12982=ORIENTED_EDGE('',*,*,#9727,.F.);
#12983=ORIENTED_EDGE('',*,*,#9687,.F.);
#12984=ORIENTED_EDGE('',*,*,#9647,.F.);
#12985=ORIENTED_EDGE('',*,*,#9648,.F.);
#12986=ORIENTED_EDGE('',*,*,#9641,.F.);
#12987=ORIENTED_EDGE('',*,*,#9642,.F.);
#12988=ORIENTED_EDGE('',*,*,#9689,.T.);
#12989=ORIENTED_EDGE('',*,*,#9723,.T.);
#12990=ORIENTED_EDGE('',*,*,#9708,.F.);
#12991=ORIENTED_EDGE('',*,*,#9855,.T.);
#12992=ORIENTED_EDGE('',*,*,#9879,.F.);
#12993=ORIENTED_EDGE('',*,*,#9822,.F.);
#12994=ORIENTED_EDGE('',*,*,#9880,.T.);
#12995=ORIENTED_EDGE('',*,*,#9856,.T.);
#12996=ORIENTED_EDGE('',*,*,#9706,.F.);
#12997=ORIENTED_EDGE('',*,*,#9824,.F.);
#12998=ORIENTED_EDGE('',*,*,#9879,.T.);
#12999=ORIENTED_EDGE('',*,*,#9857,.T.);
#13000=ORIENTED_EDGE('',*,*,#9880,.F.);
#13001=ORIENTED_EDGE('',*,*,#9823,.F.);
#13002=ORIENTED_EDGE('',*,*,#9881,.F.);
#13003=ORIENTED_EDGE('',*,*,#9882,.T.);
#13004=ORIENTED_EDGE('',*,*,#9883,.F.);
#13005=ORIENTED_EDGE('',*,*,#9884,.F.);
#13006=ORIENTED_EDGE('',*,*,#9885,.T.);
#13007=ORIENTED_EDGE('',*,*,#9886,.T.);
#13008=ORIENTED_EDGE('',*,*,#9887,.T.);
#13009=ORIENTED_EDGE('',*,*,#9885,.F.);
#13010=ORIENTED_EDGE('',*,*,#9888,.F.);
#13011=ORIENTED_EDGE('',*,*,#9889,.F.);
#13012=ORIENTED_EDGE('',*,*,#9882,.F.);
#13013=ORIENTED_EDGE('',*,*,#9890,.F.);
#13014=ORIENTED_EDGE('',*,*,#9891,.F.);
#13015=ORIENTED_EDGE('',*,*,#9892,.F.);
#13016=ORIENTED_EDGE('',*,*,#9893,.T.);
#13017=ORIENTED_EDGE('',*,*,#9894,.T.);
#13018=ORIENTED_EDGE('',*,*,#9895,.T.);
#13019=ORIENTED_EDGE('',*,*,#9896,.T.);
#13020=ORIENTED_EDGE('',*,*,#9897,.T.);
#13021=ORIENTED_EDGE('',*,*,#9898,.T.);
#13022=ORIENTED_EDGE('',*,*,#9896,.F.);
#13023=ORIENTED_EDGE('',*,*,#9899,.T.);
#13024=ORIENTED_EDGE('',*,*,#9900,.T.);
#13025=ORIENTED_EDGE('',*,*,#9893,.F.);
#13026=ORIENTED_EDGE('',*,*,#9901,.T.);
#13027=ORIENTED_EDGE('',*,*,#9902,.T.);
#13028=ORIENTED_EDGE('',*,*,#9883,.T.);
#13029=ORIENTED_EDGE('',*,*,#9889,.T.);
#13030=ORIENTED_EDGE('',*,*,#9903,.F.);
#13031=ORIENTED_EDGE('',*,*,#9887,.F.);
#13032=ORIENTED_EDGE('',*,*,#9904,.T.);
#13033=ORIENTED_EDGE('',*,*,#9905,.T.);
#13034=ORIENTED_EDGE('',*,*,#9904,.F.);
#13035=ORIENTED_EDGE('',*,*,#9886,.F.);
#13036=ORIENTED_EDGE('',*,*,#9906,.F.);
#13037=ORIENTED_EDGE('',*,*,#9907,.T.);
#13038=ORIENTED_EDGE('',*,*,#9890,.T.);
#13039=ORIENTED_EDGE('',*,*,#9881,.T.);
#13040=ORIENTED_EDGE('',*,*,#9907,.F.);
#13041=ORIENTED_EDGE('',*,*,#9908,.F.);
#13042=ORIENTED_EDGE('',*,*,#9909,.T.);
#13043=ORIENTED_EDGE('',*,*,#9894,.F.);
#13044=ORIENTED_EDGE('',*,*,#9900,.F.);
#13045=ORIENTED_EDGE('',*,*,#9910,.F.);
#13046=ORIENTED_EDGE('',*,*,#9911,.F.);
#13047=ORIENTED_EDGE('',*,*,#9912,.T.);
#13048=ORIENTED_EDGE('',*,*,#9891,.T.);
#13049=ORIENTED_EDGE('',*,*,#9892,.T.);
#13050=ORIENTED_EDGE('',*,*,#9912,.F.);
#13051=ORIENTED_EDGE('',*,*,#9897,.F.);
#13052=ORIENTED_EDGE('',*,*,#9898,.F.);
#13053=ORIENTED_EDGE('',*,*,#9913,.T.);
#13054=ORIENTED_EDGE('',*,*,#9914,.T.);
#13055=ORIENTED_EDGE('',*,*,#9913,.F.);
#13056=ORIENTED_EDGE('',*,*,#9911,.T.);
#13057=ORIENTED_EDGE('',*,*,#9905,.F.);
#13058=ORIENTED_EDGE('',*,*,#9914,.F.);
#13059=ORIENTED_EDGE('',*,*,#9906,.T.);
#13060=ORIENTED_EDGE('',*,*,#9915,.T.);
#13061=ORIENTED_EDGE('',*,*,#9908,.T.);
#13062=ORIENTED_EDGE('',*,*,#9909,.F.);
#13063=ORIENTED_EDGE('',*,*,#9915,.F.);
#13064=ORIENTED_EDGE('',*,*,#9910,.T.);
#13065=ORIENTED_EDGE('',*,*,#9899,.F.);
#13066=ORIENTED_EDGE('',*,*,#9895,.F.);
#13067=ORIENTED_EDGE('',*,*,#9901,.F.);
#13068=ORIENTED_EDGE('',*,*,#9916,.F.);
#13069=ORIENTED_EDGE('',*,*,#9902,.F.);
#13070=ORIENTED_EDGE('',*,*,#9916,.T.);
#13071=ORIENTED_EDGE('',*,*,#9903,.T.);
#13072=ORIENTED_EDGE('',*,*,#9888,.T.);
#13073=ORIENTED_EDGE('',*,*,#9884,.T.);
#13074=ORIENTED_EDGE('',*,*,#9917,.F.);
#13075=ORIENTED_EDGE('',*,*,#9918,.T.);
#13076=ORIENTED_EDGE('',*,*,#9919,.T.);
#13077=ORIENTED_EDGE('',*,*,#9918,.F.);
#13078=ORIENTED_EDGE('',*,*,#9920,.F.);
#13079=ORIENTED_EDGE('',*,*,#9921,.T.);
#13080=ORIENTED_EDGE('',*,*,#9922,.T.);
#13081=ORIENTED_EDGE('',*,*,#9921,.F.);
#13082=ORIENTED_EDGE('',*,*,#9923,.F.);
#13083=ORIENTED_EDGE('',*,*,#9924,.T.);
#13084=ORIENTED_EDGE('',*,*,#9925,.T.);
#13085=ORIENTED_EDGE('',*,*,#9924,.F.);
#13086=ORIENTED_EDGE('',*,*,#9926,.F.);
#13087=ORIENTED_EDGE('',*,*,#9927,.T.);
#13088=ORIENTED_EDGE('',*,*,#9928,.T.);
#13089=ORIENTED_EDGE('',*,*,#9927,.F.);
#13090=ORIENTED_EDGE('',*,*,#9929,.F.);
#13091=ORIENTED_EDGE('',*,*,#9930,.F.);
#13092=ORIENTED_EDGE('',*,*,#9931,.F.);
#13093=ORIENTED_EDGE('',*,*,#9932,.F.);
#13094=ORIENTED_EDGE('',*,*,#9933,.F.);
#13095=ORIENTED_EDGE('',*,*,#9934,.F.);
#13096=ORIENTED_EDGE('',*,*,#9935,.F.);
#13097=ORIENTED_EDGE('',*,*,#9936,.T.);
#13098=ORIENTED_EDGE('',*,*,#9937,.T.);
#13099=ORIENTED_EDGE('',*,*,#9938,.F.);
#13100=ORIENTED_EDGE('',*,*,#9939,.F.);
#13101=ORIENTED_EDGE('',*,*,#9940,.F.);
#13102=ORIENTED_EDGE('',*,*,#9941,.F.);
#13103=ORIENTED_EDGE('',*,*,#9942,.F.);
#13104=ORIENTED_EDGE('',*,*,#9943,.T.);
#13105=ORIENTED_EDGE('',*,*,#9944,.T.);
#13106=ORIENTED_EDGE('',*,*,#9945,.T.);
#13107=ORIENTED_EDGE('',*,*,#9946,.T.);
#13108=ORIENTED_EDGE('',*,*,#9947,.F.);
#13109=ORIENTED_EDGE('',*,*,#9948,.T.);
#13110=ORIENTED_EDGE('',*,*,#9949,.T.);
#13111=ORIENTED_EDGE('',*,*,#9950,.T.);
#13112=ORIENTED_EDGE('',*,*,#9951,.T.);
#13113=ORIENTED_EDGE('',*,*,#9952,.F.);
#13114=ORIENTED_EDGE('',*,*,#9953,.F.);
#13115=ORIENTED_EDGE('',*,*,#9954,.F.);
#13116=ORIENTED_EDGE('',*,*,#9955,.T.);
#13117=ORIENTED_EDGE('',*,*,#9935,.T.);
#13118=ORIENTED_EDGE('',*,*,#9956,.F.);
#13119=ORIENTED_EDGE('',*,*,#9957,.F.);
#13120=ORIENTED_EDGE('',*,*,#9958,.T.);
#13121=ORIENTED_EDGE('',*,*,#9954,.T.);
#13122=ORIENTED_EDGE('',*,*,#9959,.F.);
#13123=ORIENTED_EDGE('',*,*,#9960,.F.);
#13124=ORIENTED_EDGE('',*,*,#9961,.T.);
#13125=ORIENTED_EDGE('',*,*,#9957,.T.);
#13126=ORIENTED_EDGE('',*,*,#9962,.F.);
#13127=ORIENTED_EDGE('',*,*,#9963,.F.);
#13128=ORIENTED_EDGE('',*,*,#9964,.T.);
#13129=ORIENTED_EDGE('',*,*,#9960,.T.);
#13130=ORIENTED_EDGE('',*,*,#9965,.F.);
#13131=ORIENTED_EDGE('',*,*,#9949,.F.);
#13132=ORIENTED_EDGE('',*,*,#9966,.T.);
#13133=ORIENTED_EDGE('',*,*,#9963,.T.);
#13134=ORIENTED_EDGE('',*,*,#9967,.F.);
#13135=ORIENTED_EDGE('',*,*,#9968,.F.);
#13136=ORIENTED_EDGE('',*,*,#9969,.T.);
#13137=ORIENTED_EDGE('',*,*,#9947,.T.);
#13138=ORIENTED_EDGE('',*,*,#9970,.F.);
#13139=ORIENTED_EDGE('',*,*,#9971,.F.);
#13140=ORIENTED_EDGE('',*,*,#9972,.T.);
#13141=ORIENTED_EDGE('',*,*,#9968,.T.);
#13142=ORIENTED_EDGE('',*,*,#9973,.F.);
#13143=ORIENTED_EDGE('',*,*,#9974,.F.);
#13144=ORIENTED_EDGE('',*,*,#9975,.T.);
#13145=ORIENTED_EDGE('',*,*,#9971,.T.);
#13146=ORIENTED_EDGE('',*,*,#9976,.F.);
#13147=ORIENTED_EDGE('',*,*,#9977,.F.);
#13148=ORIENTED_EDGE('',*,*,#9978,.T.);
#13149=ORIENTED_EDGE('',*,*,#9974,.T.);
#13150=ORIENTED_EDGE('',*,*,#9979,.F.);
#13151=ORIENTED_EDGE('',*,*,#9937,.F.);
#13152=ORIENTED_EDGE('',*,*,#9980,.T.);
#13153=ORIENTED_EDGE('',*,*,#9977,.T.);
#13154=ORIENTED_EDGE('',*,*,#9936,.F.);
#13155=ORIENTED_EDGE('',*,*,#9955,.F.);
#13156=ORIENTED_EDGE('',*,*,#9958,.F.);
#13157=ORIENTED_EDGE('',*,*,#9961,.F.);
#13158=ORIENTED_EDGE('',*,*,#9964,.F.);
#13159=ORIENTED_EDGE('',*,*,#9966,.F.);
#13160=ORIENTED_EDGE('',*,*,#9948,.F.);
#13161=ORIENTED_EDGE('',*,*,#9969,.F.);
#13162=ORIENTED_EDGE('',*,*,#9972,.F.);
#13163=ORIENTED_EDGE('',*,*,#9975,.F.);
#13164=ORIENTED_EDGE('',*,*,#9978,.F.);
#13165=ORIENTED_EDGE('',*,*,#9980,.F.);
#13166=ORIENTED_EDGE('',*,*,#9917,.T.);
#13167=ORIENTED_EDGE('',*,*,#9920,.T.);
#13168=ORIENTED_EDGE('',*,*,#9923,.T.);
#13169=ORIENTED_EDGE('',*,*,#9926,.T.);
#13170=ORIENTED_EDGE('',*,*,#9953,.T.);
#13171=ORIENTED_EDGE('',*,*,#9934,.T.);
#13172=ORIENTED_EDGE('',*,*,#9981,.F.);
#13173=ORIENTED_EDGE('',*,*,#9982,.F.);
#13174=ORIENTED_EDGE('',*,*,#9983,.T.);
#13175=ORIENTED_EDGE('',*,*,#9979,.T.);
#13176=ORIENTED_EDGE('',*,*,#9976,.T.);
#13177=ORIENTED_EDGE('',*,*,#9973,.T.);
#13178=ORIENTED_EDGE('',*,*,#9970,.T.);
#13179=ORIENTED_EDGE('',*,*,#9967,.T.);
#13180=ORIENTED_EDGE('',*,*,#9984,.F.);
#13181=ORIENTED_EDGE('',*,*,#9985,.T.);
#13182=ORIENTED_EDGE('',*,*,#9986,.T.);
#13183=ORIENTED_EDGE('',*,*,#9950,.F.);
#13184=ORIENTED_EDGE('',*,*,#9965,.T.);
#13185=ORIENTED_EDGE('',*,*,#9962,.T.);
#13186=ORIENTED_EDGE('',*,*,#9959,.T.);
#13187=ORIENTED_EDGE('',*,*,#9956,.T.);
#13188=ORIENTED_EDGE('',*,*,#9919,.F.);
#13189=ORIENTED_EDGE('',*,*,#9922,.F.);
#13190=ORIENTED_EDGE('',*,*,#9925,.F.);
#13191=ORIENTED_EDGE('',*,*,#9928,.F.);
#13192=ORIENTED_EDGE('',*,*,#9938,.T.);
#13193=ORIENTED_EDGE('',*,*,#9983,.F.);
#13194=ORIENTED_EDGE('',*,*,#9987,.F.);
#13195=ORIENTED_EDGE('',*,*,#9988,.T.);
#13196=ORIENTED_EDGE('',*,*,#9933,.T.);
#13197=ORIENTED_EDGE('',*,*,#9989,.F.);
#13198=ORIENTED_EDGE('',*,*,#9990,.F.);
#13199=ORIENTED_EDGE('',*,*,#9981,.T.);
#13200=ORIENTED_EDGE('',*,*,#9989,.T.);
#13201=ORIENTED_EDGE('',*,*,#9932,.T.);
#13202=ORIENTED_EDGE('',*,*,#9991,.F.);
#13203=ORIENTED_EDGE('',*,*,#9952,.T.);
#13204=ORIENTED_EDGE('',*,*,#9992,.F.);
#13205=ORIENTED_EDGE('',*,*,#9993,.T.);
#13206=ORIENTED_EDGE('',*,*,#9994,.F.);
#13207=ORIENTED_EDGE('',*,*,#9995,.F.);
#13208=ORIENTED_EDGE('',*,*,#9994,.T.);
#13209=ORIENTED_EDGE('',*,*,#9996,.T.);
#13210=ORIENTED_EDGE('',*,*,#9997,.T.);
#13211=ORIENTED_EDGE('',*,*,#9943,.F.);
#13212=ORIENTED_EDGE('',*,*,#9998,.T.);
#13213=ORIENTED_EDGE('',*,*,#9929,.T.);
#13214=ORIENTED_EDGE('',*,*,#9999,.F.);
#13215=ORIENTED_EDGE('',*,*,#10000,.F.);
#13216=ORIENTED_EDGE('',*,*,#9940,.T.);
#13217=ORIENTED_EDGE('',*,*,#10001,.F.);
#13218=ORIENTED_EDGE('',*,*,#10002,.F.);
#13219=ORIENTED_EDGE('',*,*,#9999,.T.);
#13220=ORIENTED_EDGE('',*,*,#9939,.T.);
#13221=ORIENTED_EDGE('',*,*,#9988,.F.);
#13222=ORIENTED_EDGE('',*,*,#10003,.F.);
#13223=ORIENTED_EDGE('',*,*,#10001,.T.);
#13224=ORIENTED_EDGE('',*,*,#9987,.T.);
#13225=ORIENTED_EDGE('',*,*,#9982,.T.);
#13226=ORIENTED_EDGE('',*,*,#9990,.T.);
#13227=ORIENTED_EDGE('',*,*,#9995,.T.);
#13228=ORIENTED_EDGE('',*,*,#10000,.T.);
#13229=ORIENTED_EDGE('',*,*,#10002,.T.);
#13230=ORIENTED_EDGE('',*,*,#10003,.T.);
#13231=ORIENTED_EDGE('',*,*,#9946,.F.);
#13232=ORIENTED_EDGE('',*,*,#10004,.F.);
#13233=ORIENTED_EDGE('',*,*,#10005,.T.);
#13234=ORIENTED_EDGE('',*,*,#9984,.T.);
#13235=ORIENTED_EDGE('',*,*,#9945,.F.);
#13236=ORIENTED_EDGE('',*,*,#10006,.F.);
#13237=ORIENTED_EDGE('',*,*,#10007,.T.);
#13238=ORIENTED_EDGE('',*,*,#10004,.T.);
#13239=ORIENTED_EDGE('',*,*,#9944,.F.);
#13240=ORIENTED_EDGE('',*,*,#9997,.F.);
#13241=ORIENTED_EDGE('',*,*,#10008,.T.);
#13242=ORIENTED_EDGE('',*,*,#10006,.T.);
#13243=ORIENTED_EDGE('',*,*,#9951,.F.);
#13244=ORIENTED_EDGE('',*,*,#9986,.F.);
#13245=ORIENTED_EDGE('',*,*,#10009,.T.);
#13246=ORIENTED_EDGE('',*,*,#9992,.T.);
#13247=ORIENTED_EDGE('',*,*,#10005,.F.);
#13248=ORIENTED_EDGE('',*,*,#10007,.F.);
#13249=ORIENTED_EDGE('',*,*,#10008,.F.);
#13250=ORIENTED_EDGE('',*,*,#9996,.F.);
#13251=ORIENTED_EDGE('',*,*,#9993,.F.);
#13252=ORIENTED_EDGE('',*,*,#10009,.F.);
#13253=ORIENTED_EDGE('',*,*,#9985,.F.);
#13254=ORIENTED_EDGE('',*,*,#9998,.F.);
#13255=ORIENTED_EDGE('',*,*,#9942,.T.);
#13256=ORIENTED_EDGE('',*,*,#10010,.T.);
#13257=ORIENTED_EDGE('',*,*,#9930,.T.);
#13258=ORIENTED_EDGE('',*,*,#10010,.F.);
#13259=ORIENTED_EDGE('',*,*,#9941,.T.);
#13260=ORIENTED_EDGE('',*,*,#9991,.T.);
#13261=ORIENTED_EDGE('',*,*,#9931,.T.);
#13262=ORIENTED_EDGE('',*,*,#10011,.F.);
#13263=ORIENTED_EDGE('',*,*,#10012,.T.);
#13264=ORIENTED_EDGE('',*,*,#10013,.T.);
#13265=ORIENTED_EDGE('',*,*,#10012,.F.);
#13266=ORIENTED_EDGE('',*,*,#10014,.T.);
#13267=ORIENTED_EDGE('',*,*,#10015,.T.);
#13268=ORIENTED_EDGE('',*,*,#10016,.F.);
#13269=ORIENTED_EDGE('',*,*,#10015,.F.);
#13270=ORIENTED_EDGE('',*,*,#10017,.T.);
#13271=ORIENTED_EDGE('',*,*,#10018,.T.);
#13272=ORIENTED_EDGE('',*,*,#10019,.F.);
#13273=ORIENTED_EDGE('',*,*,#10018,.F.);
#13274=ORIENTED_EDGE('',*,*,#10020,.T.);
#13275=ORIENTED_EDGE('',*,*,#10021,.T.);
#13276=ORIENTED_EDGE('',*,*,#10022,.F.);
#13277=ORIENTED_EDGE('',*,*,#10021,.F.);
#13278=ORIENTED_EDGE('',*,*,#10023,.T.);
#13279=ORIENTED_EDGE('',*,*,#10024,.T.);
#13280=ORIENTED_EDGE('',*,*,#10025,.F.);
#13281=ORIENTED_EDGE('',*,*,#10024,.F.);
#13282=ORIENTED_EDGE('',*,*,#10026,.T.);
#13283=ORIENTED_EDGE('',*,*,#10027,.T.);
#13284=ORIENTED_EDGE('',*,*,#10028,.F.);
#13285=ORIENTED_EDGE('',*,*,#10027,.F.);
#13286=ORIENTED_EDGE('',*,*,#10029,.T.);
#13287=ORIENTED_EDGE('',*,*,#10030,.T.);
#13288=ORIENTED_EDGE('',*,*,#10031,.F.);
#13289=ORIENTED_EDGE('',*,*,#10030,.F.);
#13290=ORIENTED_EDGE('',*,*,#10032,.T.);
#13291=ORIENTED_EDGE('',*,*,#10033,.T.);
#13292=ORIENTED_EDGE('',*,*,#10034,.F.);
#13293=ORIENTED_EDGE('',*,*,#10033,.F.);
#13294=ORIENTED_EDGE('',*,*,#10035,.T.);
#13295=ORIENTED_EDGE('',*,*,#10036,.T.);
#13296=ORIENTED_EDGE('',*,*,#10037,.F.);
#13297=ORIENTED_EDGE('',*,*,#10036,.F.);
#13298=ORIENTED_EDGE('',*,*,#10038,.T.);
#13299=ORIENTED_EDGE('',*,*,#10039,.T.);
#13300=ORIENTED_EDGE('',*,*,#10040,.F.);
#13301=ORIENTED_EDGE('',*,*,#10039,.F.);
#13302=ORIENTED_EDGE('',*,*,#10041,.T.);
#13303=ORIENTED_EDGE('',*,*,#10042,.T.);
#13304=ORIENTED_EDGE('',*,*,#10043,.F.);
#13305=ORIENTED_EDGE('',*,*,#10042,.F.);
#13306=ORIENTED_EDGE('',*,*,#10044,.T.);
#13307=ORIENTED_EDGE('',*,*,#10045,.T.);
#13308=ORIENTED_EDGE('',*,*,#10046,.F.);
#13309=ORIENTED_EDGE('',*,*,#10045,.F.);
#13310=ORIENTED_EDGE('',*,*,#10047,.T.);
#13311=ORIENTED_EDGE('',*,*,#10048,.T.);
#13312=ORIENTED_EDGE('',*,*,#10049,.F.);
#13313=ORIENTED_EDGE('',*,*,#10048,.F.);
#13314=ORIENTED_EDGE('',*,*,#10050,.T.);
#13315=ORIENTED_EDGE('',*,*,#10051,.T.);
#13316=ORIENTED_EDGE('',*,*,#10052,.F.);
#13317=ORIENTED_EDGE('',*,*,#10051,.F.);
#13318=ORIENTED_EDGE('',*,*,#10053,.T.);
#13319=ORIENTED_EDGE('',*,*,#10054,.T.);
#13320=ORIENTED_EDGE('',*,*,#10055,.F.);
#13321=ORIENTED_EDGE('',*,*,#10054,.F.);
#13322=ORIENTED_EDGE('',*,*,#10056,.T.);
#13323=ORIENTED_EDGE('',*,*,#10057,.T.);
#13324=ORIENTED_EDGE('',*,*,#10058,.F.);
#13325=ORIENTED_EDGE('',*,*,#10057,.F.);
#13326=ORIENTED_EDGE('',*,*,#10059,.T.);
#13327=ORIENTED_EDGE('',*,*,#10060,.T.);
#13328=ORIENTED_EDGE('',*,*,#10061,.F.);
#13329=ORIENTED_EDGE('',*,*,#10060,.F.);
#13330=ORIENTED_EDGE('',*,*,#10061,.T.);
#13331=ORIENTED_EDGE('',*,*,#10056,.F.);
#13332=ORIENTED_EDGE('',*,*,#10050,.F.);
#13333=ORIENTED_EDGE('',*,*,#10044,.F.);
#13334=ORIENTED_EDGE('',*,*,#10038,.F.);
#13335=ORIENTED_EDGE('',*,*,#10032,.F.);
#13336=ORIENTED_EDGE('',*,*,#10026,.F.);
#13337=ORIENTED_EDGE('',*,*,#10020,.F.);
#13338=ORIENTED_EDGE('',*,*,#10014,.F.);
#13339=ORIENTED_EDGE('',*,*,#10013,.F.);
#13340=ORIENTED_EDGE('',*,*,#10017,.F.);
#13341=ORIENTED_EDGE('',*,*,#10023,.F.);
#13342=ORIENTED_EDGE('',*,*,#10029,.F.);
#13343=ORIENTED_EDGE('',*,*,#10035,.F.);
#13344=ORIENTED_EDGE('',*,*,#10041,.F.);
#13345=ORIENTED_EDGE('',*,*,#10047,.F.);
#13346=ORIENTED_EDGE('',*,*,#10053,.F.);
#13347=ORIENTED_EDGE('',*,*,#10059,.F.);
#13348=ORIENTED_EDGE('',*,*,#10058,.T.);
#13349=ORIENTED_EDGE('',*,*,#10055,.T.);
#13350=ORIENTED_EDGE('',*,*,#10052,.T.);
#13351=ORIENTED_EDGE('',*,*,#10049,.T.);
#13352=ORIENTED_EDGE('',*,*,#10046,.T.);
#13353=ORIENTED_EDGE('',*,*,#10043,.T.);
#13354=ORIENTED_EDGE('',*,*,#10040,.T.);
#13355=ORIENTED_EDGE('',*,*,#10037,.T.);
#13356=ORIENTED_EDGE('',*,*,#10034,.T.);
#13357=ORIENTED_EDGE('',*,*,#10031,.T.);
#13358=ORIENTED_EDGE('',*,*,#10028,.T.);
#13359=ORIENTED_EDGE('',*,*,#10025,.T.);
#13360=ORIENTED_EDGE('',*,*,#10022,.T.);
#13361=ORIENTED_EDGE('',*,*,#10019,.T.);
#13362=ORIENTED_EDGE('',*,*,#10016,.T.);
#13363=ORIENTED_EDGE('',*,*,#10011,.T.);
#13364=ORIENTED_EDGE('',*,*,#10062,.F.);
#13365=ORIENTED_EDGE('',*,*,#10063,.T.);
#13366=ORIENTED_EDGE('',*,*,#10064,.T.);
#13367=ORIENTED_EDGE('',*,*,#10063,.F.);
#13368=ORIENTED_EDGE('',*,*,#10064,.F.);
#13369=ORIENTED_EDGE('',*,*,#10062,.T.);
#13370=ORIENTED_EDGE('',*,*,#10065,.T.);
#13371=ORIENTED_EDGE('',*,*,#10066,.T.);
#13372=ORIENTED_EDGE('',*,*,#10067,.F.);
#13373=ORIENTED_EDGE('',*,*,#10068,.F.);
#13374=ORIENTED_EDGE('',*,*,#10066,.F.);
#13375=ORIENTED_EDGE('',*,*,#10069,.F.);
#13376=ORIENTED_EDGE('',*,*,#10070,.T.);
#13377=ORIENTED_EDGE('',*,*,#10071,.T.);
#13378=ORIENTED_EDGE('',*,*,#10072,.T.);
#13379=ORIENTED_EDGE('',*,*,#10070,.F.);
#13380=ORIENTED_EDGE('',*,*,#10073,.F.);
#13381=ORIENTED_EDGE('',*,*,#10074,.F.);
#13382=ORIENTED_EDGE('',*,*,#10075,.T.);
#13383=ORIENTED_EDGE('',*,*,#10076,.T.);
#13384=ORIENTED_EDGE('',*,*,#10077,.T.);
#13385=ORIENTED_EDGE('',*,*,#10075,.F.);
#13386=ORIENTED_EDGE('',*,*,#10078,.F.);
#13387=ORIENTED_EDGE('',*,*,#10079,.F.);
#13388=ORIENTED_EDGE('',*,*,#10080,.T.);
#13389=ORIENTED_EDGE('',*,*,#10081,.F.);
#13390=ORIENTED_EDGE('',*,*,#10082,.F.);
#13391=ORIENTED_EDGE('',*,*,#10080,.F.);
#13392=ORIENTED_EDGE('',*,*,#10083,.F.);
#13393=ORIENTED_EDGE('',*,*,#10084,.F.);
#13394=ORIENTED_EDGE('',*,*,#10085,.T.);
#13395=ORIENTED_EDGE('',*,*,#10086,.T.);
#13396=ORIENTED_EDGE('',*,*,#10085,.F.);
#13397=ORIENTED_EDGE('',*,*,#10069,.T.);
#13398=ORIENTED_EDGE('',*,*,#10087,.T.);
#13399=ORIENTED_EDGE('',*,*,#10067,.T.);
#13400=ORIENTED_EDGE('',*,*,#10068,.T.);
#13401=ORIENTED_EDGE('',*,*,#10087,.F.);
#13402=ORIENTED_EDGE('',*,*,#10073,.T.);
#13403=ORIENTED_EDGE('',*,*,#10077,.F.);
#13404=ORIENTED_EDGE('',*,*,#10088,.T.);
#13405=ORIENTED_EDGE('',*,*,#10089,.T.);
#13406=ORIENTED_EDGE('',*,*,#10088,.F.);
#13407=ORIENTED_EDGE('',*,*,#10076,.F.);
#13408=ORIENTED_EDGE('',*,*,#10079,.T.);
#13409=ORIENTED_EDGE('',*,*,#10090,.T.);
#13410=ORIENTED_EDGE('',*,*,#10071,.F.);
#13411=ORIENTED_EDGE('',*,*,#10072,.F.);
#13412=ORIENTED_EDGE('',*,*,#10090,.F.);
#13413=ORIENTED_EDGE('',*,*,#10083,.T.);
#13414=ORIENTED_EDGE('',*,*,#10074,.T.);
#13415=ORIENTED_EDGE('',*,*,#10091,.T.);
#13416=ORIENTED_EDGE('',*,*,#10081,.T.);
#13417=ORIENTED_EDGE('',*,*,#10082,.T.);
#13418=ORIENTED_EDGE('',*,*,#10091,.F.);
#13419=ORIENTED_EDGE('',*,*,#10078,.T.);
#13420=ORIENTED_EDGE('',*,*,#10086,.F.);
#13421=ORIENTED_EDGE('',*,*,#10065,.F.);
#13422=ORIENTED_EDGE('',*,*,#10084,.T.);
#13423=ORIENTED_EDGE('',*,*,#10089,.F.);
#13424=ORIENTED_EDGE('',*,*,#10092,.T.);
#13425=ORIENTED_EDGE('',*,*,#10093,.T.);
#13426=ORIENTED_EDGE('',*,*,#10094,.T.);
#13427=ORIENTED_EDGE('',*,*,#10095,.T.);
#13428=ORIENTED_EDGE('',*,*,#10094,.F.);
#13429=ORIENTED_EDGE('',*,*,#10092,.F.);
#13430=ORIENTED_EDGE('',*,*,#10093,.F.);
#13431=ORIENTED_EDGE('',*,*,#10096,.T.);
#13432=ORIENTED_EDGE('',*,*,#10097,.T.);
#13433=ORIENTED_EDGE('',*,*,#10096,.F.);
#13434=ORIENTED_EDGE('',*,*,#10097,.F.);
#13435=ORIENTED_EDGE('',*,*,#10095,.F.);
#13436=ORIENTED_EDGE('',*,*,#10098,.T.);
#13437=ORIENTED_EDGE('',*,*,#10099,.F.);
#13438=ORIENTED_EDGE('',*,*,#10098,.F.);
#13439=ORIENTED_EDGE('',*,*,#10099,.T.);
#13440=ORIENTED_EDGE('',*,*,#10100,.T.);
#13441=ORIENTED_EDGE('',*,*,#10101,.T.);
#13442=ORIENTED_EDGE('',*,*,#10102,.T.);
#13443=ORIENTED_EDGE('',*,*,#10103,.T.);
#13444=ORIENTED_EDGE('',*,*,#10104,.T.);
#13445=ORIENTED_EDGE('',*,*,#10105,.T.);
#13446=ORIENTED_EDGE('',*,*,#10106,.F.);
#13447=ORIENTED_EDGE('',*,*,#10101,.F.);
#13448=ORIENTED_EDGE('',*,*,#10107,.F.);
#13449=ORIENTED_EDGE('',*,*,#10108,.F.);
#13450=ORIENTED_EDGE('',*,*,#10107,.T.);
#13451=ORIENTED_EDGE('',*,*,#10100,.F.);
#13452=ORIENTED_EDGE('',*,*,#10109,.F.);
#13453=ORIENTED_EDGE('',*,*,#10110,.F.);
#13454=ORIENTED_EDGE('',*,*,#10109,.T.);
#13455=ORIENTED_EDGE('',*,*,#10105,.F.);
#13456=ORIENTED_EDGE('',*,*,#10111,.F.);
#13457=ORIENTED_EDGE('',*,*,#10112,.F.);
#13458=ORIENTED_EDGE('',*,*,#10113,.F.);
#13459=ORIENTED_EDGE('',*,*,#10111,.T.);
#13460=ORIENTED_EDGE('',*,*,#10104,.F.);
#13461=ORIENTED_EDGE('',*,*,#10114,.F.);
#13462=ORIENTED_EDGE('',*,*,#10115,.F.);
#13463=ORIENTED_EDGE('',*,*,#10114,.T.);
#13464=ORIENTED_EDGE('',*,*,#10103,.F.);
#13465=ORIENTED_EDGE('',*,*,#10116,.F.);
#13466=ORIENTED_EDGE('',*,*,#10117,.F.);
#13467=ORIENTED_EDGE('',*,*,#10118,.F.);
#13468=ORIENTED_EDGE('',*,*,#10116,.T.);
#13469=ORIENTED_EDGE('',*,*,#10102,.F.);
#13470=ORIENTED_EDGE('',*,*,#10106,.T.);
#13471=ORIENTED_EDGE('',*,*,#10119,.F.);
#13472=ORIENTED_EDGE('',*,*,#10113,.T.);
#13473=ORIENTED_EDGE('',*,*,#10120,.T.);
#13474=ORIENTED_EDGE('',*,*,#10119,.T.);
#13475=ORIENTED_EDGE('',*,*,#10108,.T.);
#13476=ORIENTED_EDGE('',*,*,#10110,.T.);
#13477=ORIENTED_EDGE('',*,*,#10115,.T.);
#13478=ORIENTED_EDGE('',*,*,#10117,.T.);
#13479=ORIENTED_EDGE('',*,*,#10118,.T.);
#13480=ORIENTED_EDGE('',*,*,#10120,.F.);
#13481=ORIENTED_EDGE('',*,*,#10112,.T.);
#13482=ORIENTED_EDGE('',*,*,#10121,.F.);
#13483=ORIENTED_EDGE('',*,*,#10122,.T.);
#13484=ORIENTED_EDGE('',*,*,#10123,.T.);
#13485=ORIENTED_EDGE('',*,*,#10124,.T.);
#13486=ORIENTED_EDGE('',*,*,#10125,.F.);
#13487=ORIENTED_EDGE('',*,*,#10126,.F.);
#13488=ORIENTED_EDGE('',*,*,#10127,.T.);
#13489=ORIENTED_EDGE('',*,*,#10128,.T.);
#13490=ORIENTED_EDGE('',*,*,#10129,.T.);
#13491=ORIENTED_EDGE('',*,*,#10130,.T.);
#13492=ORIENTED_EDGE('',*,*,#10122,.F.);
#13493=ORIENTED_EDGE('',*,*,#10131,.F.);
#13494=ORIENTED_EDGE('',*,*,#10132,.T.);
#13495=ORIENTED_EDGE('',*,*,#10133,.T.);
#13496=ORIENTED_EDGE('',*,*,#10134,.T.);
#13497=ORIENTED_EDGE('',*,*,#10132,.F.);
#13498=ORIENTED_EDGE('',*,*,#10135,.F.);
#13499=ORIENTED_EDGE('',*,*,#10136,.T.);
#13500=ORIENTED_EDGE('',*,*,#10137,.F.);
#13501=ORIENTED_EDGE('',*,*,#10136,.F.);
#13502=ORIENTED_EDGE('',*,*,#10138,.F.);
#13503=ORIENTED_EDGE('',*,*,#10139,.T.);
#13504=ORIENTED_EDGE('',*,*,#10140,.F.);
#13505=ORIENTED_EDGE('',*,*,#10139,.F.);
#13506=ORIENTED_EDGE('',*,*,#10141,.F.);
#13507=ORIENTED_EDGE('',*,*,#10142,.T.);
#13508=ORIENTED_EDGE('',*,*,#10143,.F.);
#13509=ORIENTED_EDGE('',*,*,#10142,.F.);
#13510=ORIENTED_EDGE('',*,*,#10144,.F.);
#13511=ORIENTED_EDGE('',*,*,#10145,.T.);
#13512=ORIENTED_EDGE('',*,*,#10146,.F.);
#13513=ORIENTED_EDGE('',*,*,#10145,.F.);
#13514=ORIENTED_EDGE('',*,*,#10147,.F.);
#13515=ORIENTED_EDGE('',*,*,#10148,.F.);
#13516=ORIENTED_EDGE('',*,*,#10149,.T.);
#13517=ORIENTED_EDGE('',*,*,#10150,.T.);
#13518=ORIENTED_EDGE('',*,*,#10149,.F.);
#13519=ORIENTED_EDGE('',*,*,#10151,.F.);
#13520=ORIENTED_EDGE('',*,*,#10152,.T.);
#13521=ORIENTED_EDGE('',*,*,#10153,.T.);
#13522=ORIENTED_EDGE('',*,*,#10154,.T.);
#13523=ORIENTED_EDGE('',*,*,#10155,.T.);
#13524=ORIENTED_EDGE('',*,*,#10156,.T.);
#13525=ORIENTED_EDGE('',*,*,#10157,.T.);
#13526=ORIENTED_EDGE('',*,*,#10158,.F.);
#13527=ORIENTED_EDGE('',*,*,#10159,.T.);
#13528=ORIENTED_EDGE('',*,*,#10160,.T.);
#13529=ORIENTED_EDGE('',*,*,#10153,.F.);
#13530=ORIENTED_EDGE('',*,*,#10161,.T.);
#13531=ORIENTED_EDGE('',*,*,#10162,.T.);
#13532=ORIENTED_EDGE('',*,*,#10163,.T.);
#13533=ORIENTED_EDGE('',*,*,#10164,.T.);
#13534=ORIENTED_EDGE('',*,*,#10165,.T.);
#13535=ORIENTED_EDGE('',*,*,#10159,.F.);
#13536=ORIENTED_EDGE('',*,*,#10166,.T.);
#13537=ORIENTED_EDGE('',*,*,#10167,.T.);
#13538=ORIENTED_EDGE('',*,*,#10168,.T.);
#13539=ORIENTED_EDGE('',*,*,#10167,.F.);
#13540=ORIENTED_EDGE('',*,*,#10169,.T.);
#13541=ORIENTED_EDGE('',*,*,#10170,.T.);
#13542=ORIENTED_EDGE('',*,*,#10171,.T.);
#13543=ORIENTED_EDGE('',*,*,#10172,.F.);
#13544=ORIENTED_EDGE('',*,*,#10173,.T.);
#13545=ORIENTED_EDGE('',*,*,#10174,.F.);
#13546=ORIENTED_EDGE('',*,*,#10175,.T.);
#13547=ORIENTED_EDGE('',*,*,#10176,.F.);
#13548=ORIENTED_EDGE('',*,*,#10177,.T.);
#13549=ORIENTED_EDGE('',*,*,#10170,.F.);
#13550=ORIENTED_EDGE('',*,*,#10178,.F.);
#13551=ORIENTED_EDGE('',*,*,#10179,.F.);
#13552=ORIENTED_EDGE('',*,*,#10180,.T.);
#13553=ORIENTED_EDGE('',*,*,#10181,.T.);
#13554=ORIENTED_EDGE('',*,*,#10182,.T.);
#13555=ORIENTED_EDGE('',*,*,#10181,.F.);
#13556=ORIENTED_EDGE('',*,*,#10183,.T.);
#13557=ORIENTED_EDGE('',*,*,#10184,.F.);
#13558=ORIENTED_EDGE('',*,*,#10185,.T.);
#13559=ORIENTED_EDGE('',*,*,#10186,.T.);
#13560=ORIENTED_EDGE('',*,*,#10187,.F.);
#13561=ORIENTED_EDGE('',*,*,#10186,.F.);
#13562=ORIENTED_EDGE('',*,*,#10188,.T.);
#13563=ORIENTED_EDGE('',*,*,#10189,.T.);
#13564=ORIENTED_EDGE('',*,*,#10190,.T.);
#13565=ORIENTED_EDGE('',*,*,#10189,.F.);
#13566=ORIENTED_EDGE('',*,*,#10191,.F.);
#13567=ORIENTED_EDGE('',*,*,#10192,.F.);
#13568=ORIENTED_EDGE('',*,*,#10193,.F.);
#13569=ORIENTED_EDGE('',*,*,#10194,.F.);
#13570=ORIENTED_EDGE('',*,*,#10195,.F.);
#13571=ORIENTED_EDGE('',*,*,#10196,.F.);
#13572=ORIENTED_EDGE('',*,*,#10197,.F.);
#13573=ORIENTED_EDGE('',*,*,#10198,.F.);
#13574=ORIENTED_EDGE('',*,*,#10199,.F.);
#13575=ORIENTED_EDGE('',*,*,#10200,.F.);
#13576=ORIENTED_EDGE('',*,*,#10201,.F.);
#13577=ORIENTED_EDGE('',*,*,#10202,.F.);
#13578=ORIENTED_EDGE('',*,*,#10203,.F.);
#13579=ORIENTED_EDGE('',*,*,#10204,.F.);
#13580=ORIENTED_EDGE('',*,*,#10205,.F.);
#13581=ORIENTED_EDGE('',*,*,#10206,.F.);
#13582=ORIENTED_EDGE('',*,*,#10207,.F.);
#13583=ORIENTED_EDGE('',*,*,#10208,.F.);
#13584=ORIENTED_EDGE('',*,*,#10209,.F.);
#13585=ORIENTED_EDGE('',*,*,#10210,.F.);
#13586=ORIENTED_EDGE('',*,*,#10211,.F.);
#13587=ORIENTED_EDGE('',*,*,#10212,.F.);
#13588=ORIENTED_EDGE('',*,*,#10213,.F.);
#13589=ORIENTED_EDGE('',*,*,#10214,.F.);
#13590=ORIENTED_EDGE('',*,*,#10215,.T.);
#13591=ORIENTED_EDGE('',*,*,#10216,.T.);
#13592=ORIENTED_EDGE('',*,*,#10217,.T.);
#13593=ORIENTED_EDGE('',*,*,#10218,.T.);
#13594=ORIENTED_EDGE('',*,*,#10219,.F.);
#13595=ORIENTED_EDGE('',*,*,#10220,.T.);
#13596=ORIENTED_EDGE('',*,*,#10221,.T.);
#13597=ORIENTED_EDGE('',*,*,#10222,.F.);
#13598=ORIENTED_EDGE('',*,*,#10221,.F.);
#13599=ORIENTED_EDGE('',*,*,#10223,.T.);
#13600=ORIENTED_EDGE('',*,*,#10224,.T.);
#13601=ORIENTED_EDGE('',*,*,#10225,.F.);
#13602=ORIENTED_EDGE('',*,*,#10224,.F.);
#13603=ORIENTED_EDGE('',*,*,#10226,.T.);
#13604=ORIENTED_EDGE('',*,*,#10227,.T.);
#13605=ORIENTED_EDGE('',*,*,#10228,.F.);
#13606=ORIENTED_EDGE('',*,*,#10227,.F.);
#13607=ORIENTED_EDGE('',*,*,#10229,.T.);
#13608=ORIENTED_EDGE('',*,*,#10230,.T.);
#13609=ORIENTED_EDGE('',*,*,#10231,.F.);
#13610=ORIENTED_EDGE('',*,*,#10230,.F.);
#13611=ORIENTED_EDGE('',*,*,#10232,.F.);
#13612=ORIENTED_EDGE('',*,*,#10233,.T.);
#13613=ORIENTED_EDGE('',*,*,#10234,.T.);
#13614=ORIENTED_EDGE('',*,*,#10233,.F.);
#13615=ORIENTED_EDGE('',*,*,#10235,.F.);
#13616=ORIENTED_EDGE('',*,*,#10236,.F.);
#13617=ORIENTED_EDGE('',*,*,#10237,.F.);
#13618=ORIENTED_EDGE('',*,*,#10238,.F.);
#13619=ORIENTED_EDGE('',*,*,#10239,.F.);
#13620=ORIENTED_EDGE('',*,*,#10240,.F.);
#13621=ORIENTED_EDGE('',*,*,#10241,.F.);
#13622=ORIENTED_EDGE('',*,*,#10242,.F.);
#13623=ORIENTED_EDGE('',*,*,#10200,.T.);
#13624=ORIENTED_EDGE('',*,*,#10243,.F.);
#13625=ORIENTED_EDGE('',*,*,#10241,.T.);
#13626=ORIENTED_EDGE('',*,*,#10244,.F.);
#13627=ORIENTED_EDGE('',*,*,#10245,.F.);
#13628=ORIENTED_EDGE('',*,*,#10246,.F.);
#13629=ORIENTED_EDGE('',*,*,#10247,.F.);
#13630=ORIENTED_EDGE('',*,*,#10248,.F.);
#13631=ORIENTED_EDGE('',*,*,#10249,.T.);
#13632=ORIENTED_EDGE('',*,*,#10250,.T.);
#13633=ORIENTED_EDGE('',*,*,#10251,.T.);
#13634=ORIENTED_EDGE('',*,*,#10252,.T.);
#13635=ORIENTED_EDGE('',*,*,#10253,.T.);
#13636=ORIENTED_EDGE('',*,*,#10254,.T.);
#13637=ORIENTED_EDGE('',*,*,#10255,.T.);
#13638=ORIENTED_EDGE('',*,*,#10256,.T.);
#13639=ORIENTED_EDGE('',*,*,#10257,.T.);
#13640=ORIENTED_EDGE('',*,*,#10258,.T.);
#13641=ORIENTED_EDGE('',*,*,#10215,.F.);
#13642=ORIENTED_EDGE('',*,*,#10259,.F.);
#13643=ORIENTED_EDGE('',*,*,#10260,.T.);
#13644=ORIENTED_EDGE('',*,*,#10261,.T.);
#13645=ORIENTED_EDGE('',*,*,#10216,.F.);
#13646=ORIENTED_EDGE('',*,*,#10258,.F.);
#13647=ORIENTED_EDGE('',*,*,#10262,.T.);
#13648=ORIENTED_EDGE('',*,*,#10263,.T.);
#13649=ORIENTED_EDGE('',*,*,#10264,.T.);
#13650=ORIENTED_EDGE('',*,*,#10265,.T.);
#13651=ORIENTED_EDGE('',*,*,#10266,.T.);
#13652=ORIENTED_EDGE('',*,*,#10267,.T.);
#13653=ORIENTED_EDGE('',*,*,#10268,.T.);
#13654=ORIENTED_EDGE('',*,*,#10269,.T.);
#13655=ORIENTED_EDGE('',*,*,#10270,.T.);
#13656=ORIENTED_EDGE('',*,*,#10271,.F.);
#13657=ORIENTED_EDGE('',*,*,#10272,.T.);
#13658=ORIENTED_EDGE('',*,*,#10273,.T.);
#13659=ORIENTED_EDGE('',*,*,#10274,.T.);
#13660=ORIENTED_EDGE('',*,*,#10275,.T.);
#13661=ORIENTED_EDGE('',*,*,#10270,.F.);
#13662=ORIENTED_EDGE('',*,*,#10276,.T.);
#13663=ORIENTED_EDGE('',*,*,#10274,.F.);
#13664=ORIENTED_EDGE('',*,*,#10277,.T.);
#13665=ORIENTED_EDGE('',*,*,#10278,.F.);
#13666=ORIENTED_EDGE('',*,*,#10279,.F.);
#13667=ORIENTED_EDGE('',*,*,#10280,.F.);
#13668=ORIENTED_EDGE('',*,*,#10281,.F.);
#13669=ORIENTED_EDGE('',*,*,#10282,.T.);
#13670=ORIENTED_EDGE('',*,*,#10283,.T.);
#13671=ORIENTED_EDGE('',*,*,#10284,.T.);
#13672=ORIENTED_EDGE('',*,*,#10285,.F.);
#13673=ORIENTED_EDGE('',*,*,#10266,.F.);
#13674=ORIENTED_EDGE('',*,*,#10286,.T.);
#13675=ORIENTED_EDGE('',*,*,#10287,.T.);
#13676=ORIENTED_EDGE('',*,*,#10288,.T.);
#13677=ORIENTED_EDGE('',*,*,#10271,.T.);
#13678=ORIENTED_EDGE('',*,*,#10275,.F.);
#13679=ORIENTED_EDGE('',*,*,#10289,.T.);
#13680=ORIENTED_EDGE('',*,*,#10290,.T.);
#13681=ORIENTED_EDGE('',*,*,#10289,.F.);
#13682=ORIENTED_EDGE('',*,*,#10276,.F.);
#13683=ORIENTED_EDGE('',*,*,#10291,.F.);
#13684=ORIENTED_EDGE('',*,*,#10292,.T.);
#13685=ORIENTED_EDGE('',*,*,#10293,.F.);
#13686=ORIENTED_EDGE('',*,*,#10292,.F.);
#13687=ORIENTED_EDGE('',*,*,#10294,.F.);
#13688=ORIENTED_EDGE('',*,*,#10295,.T.);
#13689=ORIENTED_EDGE('',*,*,#10296,.F.);
#13690=ORIENTED_EDGE('',*,*,#10295,.F.);
#13691=ORIENTED_EDGE('',*,*,#10297,.F.);
#13692=ORIENTED_EDGE('',*,*,#10298,.T.);
#13693=ORIENTED_EDGE('',*,*,#10299,.F.);
#13694=ORIENTED_EDGE('',*,*,#10298,.F.);
#13695=ORIENTED_EDGE('',*,*,#10300,.F.);
#13696=ORIENTED_EDGE('',*,*,#10301,.T.);
#13697=ORIENTED_EDGE('',*,*,#10302,.F.);
#13698=ORIENTED_EDGE('',*,*,#10301,.F.);
#13699=ORIENTED_EDGE('',*,*,#10303,.F.);
#13700=ORIENTED_EDGE('',*,*,#10304,.T.);
#13701=ORIENTED_EDGE('',*,*,#10305,.T.);
#13702=ORIENTED_EDGE('',*,*,#10306,.T.);
#13703=ORIENTED_EDGE('',*,*,#10307,.T.);
#13704=ORIENTED_EDGE('',*,*,#10308,.T.);
#13705=ORIENTED_EDGE('',*,*,#10309,.T.);
#13706=ORIENTED_EDGE('',*,*,#10308,.F.);
#13707=ORIENTED_EDGE('',*,*,#10310,.T.);
#13708=ORIENTED_EDGE('',*,*,#10311,.T.);
#13709=ORIENTED_EDGE('',*,*,#10312,.T.);
#13710=ORIENTED_EDGE('',*,*,#10304,.F.);
#13711=ORIENTED_EDGE('',*,*,#10313,.F.);
#13712=ORIENTED_EDGE('',*,*,#10314,.T.);
#13713=ORIENTED_EDGE('',*,*,#10315,.F.);
#13714=ORIENTED_EDGE('',*,*,#10314,.F.);
#13715=ORIENTED_EDGE('',*,*,#10316,.F.);
#13716=ORIENTED_EDGE('',*,*,#10317,.T.);
#13717=ORIENTED_EDGE('',*,*,#10318,.T.);
#13718=ORIENTED_EDGE('',*,*,#10317,.F.);
#13719=ORIENTED_EDGE('',*,*,#10309,.F.);
#13720=ORIENTED_EDGE('',*,*,#10319,.T.);
#13721=ORIENTED_EDGE('',*,*,#10320,.T.);
#13722=ORIENTED_EDGE('',*,*,#10319,.F.);
#13723=ORIENTED_EDGE('',*,*,#10321,.F.);
#13724=ORIENTED_EDGE('',*,*,#10322,.T.);
#13725=ORIENTED_EDGE('',*,*,#10323,.T.);
#13726=ORIENTED_EDGE('',*,*,#10322,.F.);
#13727=ORIENTED_EDGE('',*,*,#10324,.F.);
#13728=ORIENTED_EDGE('',*,*,#10325,.T.);
#13729=ORIENTED_EDGE('',*,*,#10326,.T.);
#13730=ORIENTED_EDGE('',*,*,#10325,.F.);
#13731=ORIENTED_EDGE('',*,*,#10327,.F.);
#13732=ORIENTED_EDGE('',*,*,#10328,.T.);
#13733=ORIENTED_EDGE('',*,*,#10329,.T.);
#13734=ORIENTED_EDGE('',*,*,#10328,.F.);
#13735=ORIENTED_EDGE('',*,*,#10330,.F.);
#13736=ORIENTED_EDGE('',*,*,#10331,.T.);
#13737=ORIENTED_EDGE('',*,*,#10332,.T.);
#13738=ORIENTED_EDGE('',*,*,#10331,.F.);
#13739=ORIENTED_EDGE('',*,*,#10333,.F.);
#13740=ORIENTED_EDGE('',*,*,#10334,.T.);
#13741=ORIENTED_EDGE('',*,*,#10335,.T.);
#13742=ORIENTED_EDGE('',*,*,#10334,.F.);
#13743=ORIENTED_EDGE('',*,*,#10336,.F.);
#13744=ORIENTED_EDGE('',*,*,#10337,.T.);
#13745=ORIENTED_EDGE('',*,*,#10338,.T.);
#13746=ORIENTED_EDGE('',*,*,#10337,.F.);
#13747=ORIENTED_EDGE('',*,*,#10339,.T.);
#13748=ORIENTED_EDGE('',*,*,#10340,.F.);
#13749=ORIENTED_EDGE('',*,*,#10341,.T.);
#13750=ORIENTED_EDGE('',*,*,#10342,.F.);
#13751=ORIENTED_EDGE('',*,*,#10134,.F.);
#13752=ORIENTED_EDGE('',*,*,#10343,.T.);
#13753=ORIENTED_EDGE('',*,*,#10344,.F.);
#13754=ORIENTED_EDGE('',*,*,#10345,.F.);
#13755=ORIENTED_EDGE('',*,*,#10343,.F.);
#13756=ORIENTED_EDGE('',*,*,#10133,.F.);
#13757=ORIENTED_EDGE('',*,*,#10346,.T.);
#13758=ORIENTED_EDGE('',*,*,#10347,.F.);
#13759=ORIENTED_EDGE('',*,*,#10348,.F.);
#13760=ORIENTED_EDGE('',*,*,#10349,.T.);
#13761=ORIENTED_EDGE('',*,*,#10350,.F.);
#13762=ORIENTED_EDGE('',*,*,#10351,.F.);
#13763=ORIENTED_EDGE('',*,*,#10352,.T.);
#13764=ORIENTED_EDGE('',*,*,#10344,.T.);
#13765=ORIENTED_EDGE('',*,*,#10345,.T.);
#13766=ORIENTED_EDGE('',*,*,#10352,.F.);
#13767=ORIENTED_EDGE('',*,*,#10353,.F.);
#13768=ORIENTED_EDGE('',*,*,#10354,.F.);
#13769=ORIENTED_EDGE('',*,*,#10355,.T.);
#13770=ORIENTED_EDGE('',*,*,#10350,.T.);
#13771=ORIENTED_EDGE('',*,*,#10351,.T.);
#13772=ORIENTED_EDGE('',*,*,#10355,.F.);
#13773=ORIENTED_EDGE('',*,*,#10356,.T.);
#13774=ORIENTED_EDGE('',*,*,#10357,.T.);
#13775=ORIENTED_EDGE('',*,*,#10358,.T.);
#13776=ORIENTED_EDGE('',*,*,#10359,.T.);
#13777=ORIENTED_EDGE('',*,*,#10360,.T.);
#13778=ORIENTED_EDGE('',*,*,#10361,.T.);
#13779=ORIENTED_EDGE('',*,*,#10362,.T.);
#13780=ORIENTED_EDGE('',*,*,#10363,.T.);
#13781=ORIENTED_EDGE('',*,*,#10364,.T.);
#13782=ORIENTED_EDGE('',*,*,#10365,.F.);
#13783=ORIENTED_EDGE('',*,*,#10366,.F.);
#13784=ORIENTED_EDGE('',*,*,#10367,.T.);
#13785=ORIENTED_EDGE('',*,*,#10368,.T.);
#13786=ORIENTED_EDGE('',*,*,#10369,.T.);
#13787=ORIENTED_EDGE('',*,*,#10370,.T.);
#13788=ORIENTED_EDGE('',*,*,#10371,.T.);
#13789=ORIENTED_EDGE('',*,*,#10372,.T.);
#13790=ORIENTED_EDGE('',*,*,#10373,.T.);
#13791=ORIENTED_EDGE('',*,*,#10374,.T.);
#13792=ORIENTED_EDGE('',*,*,#10375,.T.);
#13793=ORIENTED_EDGE('',*,*,#10376,.T.);
#13794=ORIENTED_EDGE('',*,*,#10377,.T.);
#13795=ORIENTED_EDGE('',*,*,#10378,.F.);
#13796=ORIENTED_EDGE('',*,*,#10377,.F.);
#13797=ORIENTED_EDGE('',*,*,#10379,.T.);
#13798=ORIENTED_EDGE('',*,*,#10380,.T.);
#13799=ORIENTED_EDGE('',*,*,#10381,.F.);
#13800=ORIENTED_EDGE('',*,*,#10380,.F.);
#13801=ORIENTED_EDGE('',*,*,#10353,.T.);
#13802=ORIENTED_EDGE('',*,*,#10354,.T.);
#13803=ORIENTED_EDGE('',*,*,#10382,.T.);
#13804=ORIENTED_EDGE('',*,*,#10383,.F.);
#13805=ORIENTED_EDGE('',*,*,#10382,.F.);
#13806=ORIENTED_EDGE('',*,*,#10384,.T.);
#13807=ORIENTED_EDGE('',*,*,#10385,.T.);
#13808=ORIENTED_EDGE('',*,*,#10386,.F.);
#13809=ORIENTED_EDGE('',*,*,#10387,.F.);
#13810=ORIENTED_EDGE('',*,*,#10385,.F.);
#13811=ORIENTED_EDGE('',*,*,#10388,.F.);
#13812=ORIENTED_EDGE('',*,*,#10389,.T.);
#13813=ORIENTED_EDGE('',*,*,#10390,.F.);
#13814=ORIENTED_EDGE('',*,*,#10391,.F.);
#13815=ORIENTED_EDGE('',*,*,#10392,.T.);
#13816=ORIENTED_EDGE('',*,*,#10386,.T.);
#13817=ORIENTED_EDGE('',*,*,#10387,.T.);
#13818=ORIENTED_EDGE('',*,*,#10392,.F.);
#13819=ORIENTED_EDGE('',*,*,#10393,.F.);
#13820=ORIENTED_EDGE('',*,*,#10394,.F.);
#13821=ORIENTED_EDGE('',*,*,#10395,.F.);
#13822=ORIENTED_EDGE('',*,*,#10396,.F.);
#13823=ORIENTED_EDGE('',*,*,#10127,.F.);
#13824=ORIENTED_EDGE('',*,*,#10395,.T.);
#13825=ORIENTED_EDGE('',*,*,#10397,.T.);
#13826=ORIENTED_EDGE('',*,*,#10398,.F.);
#13827=ORIENTED_EDGE('',*,*,#10399,.T.);
#13828=ORIENTED_EDGE('',*,*,#10400,.F.);
#13829=ORIENTED_EDGE('',*,*,#10401,.F.);
#13830=ORIENTED_EDGE('',*,*,#10402,.F.);
#13831=ORIENTED_EDGE('',*,*,#10403,.F.);
#13832=ORIENTED_EDGE('',*,*,#10404,.F.);
#13833=ORIENTED_EDGE('',*,*,#10405,.T.);
#13834=ORIENTED_EDGE('',*,*,#10371,.F.);
#13835=ORIENTED_EDGE('',*,*,#10406,.F.);
#13836=ORIENTED_EDGE('',*,*,#10369,.F.);
#13837=ORIENTED_EDGE('',*,*,#10407,.F.);
#13838=ORIENTED_EDGE('',*,*,#10408,.F.);
#13839=ORIENTED_EDGE('',*,*,#10409,.F.);
#13840=ORIENTED_EDGE('',*,*,#10410,.F.);
#13841=ORIENTED_EDGE('',*,*,#10408,.T.);
#13842=ORIENTED_EDGE('',*,*,#10411,.T.);
#13843=ORIENTED_EDGE('',*,*,#10412,.T.);
#13844=ORIENTED_EDGE('',*,*,#10413,.F.);
#13845=ORIENTED_EDGE('',*,*,#10414,.F.);
#13846=ORIENTED_EDGE('',*,*,#10415,.F.);
#13847=ORIENTED_EDGE('',*,*,#10416,.F.);
#13848=ORIENTED_EDGE('',*,*,#10414,.T.);
#13849=ORIENTED_EDGE('',*,*,#10417,.T.);
#13850=ORIENTED_EDGE('',*,*,#10418,.F.);
#13851=ORIENTED_EDGE('',*,*,#10419,.T.);
#13852=ORIENTED_EDGE('',*,*,#10420,.F.);
#13853=ORIENTED_EDGE('',*,*,#10421,.F.);
#13854=ORIENTED_EDGE('',*,*,#10422,.F.);
#13855=ORIENTED_EDGE('',*,*,#10423,.F.);
#13856=ORIENTED_EDGE('',*,*,#10424,.F.);
#13857=ORIENTED_EDGE('',*,*,#10425,.F.);
#13858=ORIENTED_EDGE('',*,*,#10426,.F.);
#13859=ORIENTED_EDGE('',*,*,#10427,.F.);
#13860=ORIENTED_EDGE('',*,*,#10428,.F.);
#13861=ORIENTED_EDGE('',*,*,#10429,.F.);
#13862=ORIENTED_EDGE('',*,*,#10430,.F.);
#13863=ORIENTED_EDGE('',*,*,#10431,.F.);
#13864=ORIENTED_EDGE('',*,*,#10432,.F.);
#13865=ORIENTED_EDGE('',*,*,#10433,.F.);
#13866=ORIENTED_EDGE('',*,*,#10434,.F.);
#13867=ORIENTED_EDGE('',*,*,#10435,.F.);
#13868=ORIENTED_EDGE('',*,*,#10436,.F.);
#13869=ORIENTED_EDGE('',*,*,#10437,.F.);
#13870=ORIENTED_EDGE('',*,*,#10438,.F.);
#13871=ORIENTED_EDGE('',*,*,#10439,.F.);
#13872=ORIENTED_EDGE('',*,*,#10440,.F.);
#13873=ORIENTED_EDGE('',*,*,#10441,.F.);
#13874=ORIENTED_EDGE('',*,*,#10442,.F.);
#13875=ORIENTED_EDGE('',*,*,#10443,.F.);
#13876=ORIENTED_EDGE('',*,*,#10444,.F.);
#13877=ORIENTED_EDGE('',*,*,#10445,.F.);
#13878=ORIENTED_EDGE('',*,*,#10446,.F.);
#13879=ORIENTED_EDGE('',*,*,#10447,.F.);
#13880=ORIENTED_EDGE('',*,*,#10448,.T.);
#13881=ORIENTED_EDGE('',*,*,#10449,.T.);
#13882=ORIENTED_EDGE('',*,*,#10450,.T.);
#13883=ORIENTED_EDGE('',*,*,#10451,.T.);
#13884=ORIENTED_EDGE('',*,*,#10452,.T.);
#13885=ORIENTED_EDGE('',*,*,#10453,.T.);
#13886=ORIENTED_EDGE('',*,*,#10454,.T.);
#13887=ORIENTED_EDGE('',*,*,#10388,.T.);
#13888=ORIENTED_EDGE('',*,*,#10455,.T.);
#13889=ORIENTED_EDGE('',*,*,#10456,.T.);
#13890=ORIENTED_EDGE('',*,*,#10457,.T.);
#13891=ORIENTED_EDGE('',*,*,#10458,.T.);
#13892=ORIENTED_EDGE('',*,*,#10459,.T.);
#13893=ORIENTED_EDGE('',*,*,#10460,.T.);
#13894=ORIENTED_EDGE('',*,*,#10461,.T.);
#13895=ORIENTED_EDGE('',*,*,#10462,.T.);
#13896=ORIENTED_EDGE('',*,*,#10463,.T.);
#13897=ORIENTED_EDGE('',*,*,#10464,.T.);
#13898=ORIENTED_EDGE('',*,*,#10465,.T.);
#13899=ORIENTED_EDGE('',*,*,#10466,.T.);
#13900=ORIENTED_EDGE('',*,*,#10467,.T.);
#13901=ORIENTED_EDGE('',*,*,#10468,.T.);
#13902=ORIENTED_EDGE('',*,*,#10469,.T.);
#13903=ORIENTED_EDGE('',*,*,#10470,.T.);
#13904=ORIENTED_EDGE('',*,*,#10471,.T.);
#13905=ORIENTED_EDGE('',*,*,#10472,.T.);
#13906=ORIENTED_EDGE('',*,*,#10473,.T.);
#13907=ORIENTED_EDGE('',*,*,#10474,.T.);
#13908=ORIENTED_EDGE('',*,*,#10475,.T.);
#13909=ORIENTED_EDGE('',*,*,#10476,.F.);
#13910=ORIENTED_EDGE('',*,*,#10427,.T.);
#13911=ORIENTED_EDGE('',*,*,#10477,.F.);
#13912=ORIENTED_EDGE('',*,*,#10478,.T.);
#13913=ORIENTED_EDGE('',*,*,#10479,.F.);
#13914=ORIENTED_EDGE('',*,*,#10428,.T.);
#13915=ORIENTED_EDGE('',*,*,#10476,.T.);
#13916=ORIENTED_EDGE('',*,*,#10480,.T.);
#13917=ORIENTED_EDGE('',*,*,#10481,.F.);
#13918=ORIENTED_EDGE('',*,*,#10429,.T.);
#13919=ORIENTED_EDGE('',*,*,#10479,.T.);
#13920=ORIENTED_EDGE('',*,*,#10482,.T.);
#13921=ORIENTED_EDGE('',*,*,#10483,.F.);
#13922=ORIENTED_EDGE('',*,*,#10424,.T.);
#13923=ORIENTED_EDGE('',*,*,#10481,.T.);
#13924=ORIENTED_EDGE('',*,*,#10484,.T.);
#13925=ORIENTED_EDGE('',*,*,#10485,.F.);
#13926=ORIENTED_EDGE('',*,*,#10425,.T.);
#13927=ORIENTED_EDGE('',*,*,#10483,.T.);
#13928=ORIENTED_EDGE('',*,*,#10486,.T.);
#13929=ORIENTED_EDGE('',*,*,#10477,.T.);
#13930=ORIENTED_EDGE('',*,*,#10426,.T.);
#13931=ORIENTED_EDGE('',*,*,#10485,.T.);
#13932=ORIENTED_EDGE('',*,*,#10487,.F.);
#13933=ORIENTED_EDGE('',*,*,#10488,.T.);
#13934=ORIENTED_EDGE('',*,*,#10489,.T.);
#13935=ORIENTED_EDGE('',*,*,#10490,.F.);
#13936=ORIENTED_EDGE('',*,*,#10491,.F.);
#13937=ORIENTED_EDGE('',*,*,#10492,.T.);
#13938=ORIENTED_EDGE('',*,*,#10493,.F.);
#13939=ORIENTED_EDGE('',*,*,#10489,.F.);
#13940=ORIENTED_EDGE('',*,*,#10494,.T.);
#13941=ORIENTED_EDGE('',*,*,#10495,.F.);
#13942=ORIENTED_EDGE('',*,*,#10492,.F.);
#13943=ORIENTED_EDGE('',*,*,#10496,.T.);
#13944=ORIENTED_EDGE('',*,*,#10497,.F.);
#13945=ORIENTED_EDGE('',*,*,#10498,.F.);
#13946=ORIENTED_EDGE('',*,*,#10499,.F.);
#13947=ORIENTED_EDGE('',*,*,#10500,.F.);
#13948=ORIENTED_EDGE('',*,*,#10432,.T.);
#13949=ORIENTED_EDGE('',*,*,#10501,.F.);
#13950=ORIENTED_EDGE('',*,*,#10502,.F.);
#13951=ORIENTED_EDGE('',*,*,#10501,.T.);
#13952=ORIENTED_EDGE('',*,*,#10431,.T.);
#13953=ORIENTED_EDGE('',*,*,#10503,.F.);
#13954=ORIENTED_EDGE('',*,*,#10504,.F.);
#13955=ORIENTED_EDGE('',*,*,#10503,.T.);
#13956=ORIENTED_EDGE('',*,*,#10430,.T.);
#13957=ORIENTED_EDGE('',*,*,#10505,.F.);
#13958=ORIENTED_EDGE('',*,*,#10506,.F.);
#13959=ORIENTED_EDGE('',*,*,#10505,.T.);
#13960=ORIENTED_EDGE('',*,*,#10435,.T.);
#13961=ORIENTED_EDGE('',*,*,#10507,.F.);
#13962=ORIENTED_EDGE('',*,*,#10508,.F.);
#13963=ORIENTED_EDGE('',*,*,#10507,.T.);
#13964=ORIENTED_EDGE('',*,*,#10434,.T.);
#13965=ORIENTED_EDGE('',*,*,#10509,.F.);
#13966=ORIENTED_EDGE('',*,*,#10510,.F.);
#13967=ORIENTED_EDGE('',*,*,#10509,.T.);
#13968=ORIENTED_EDGE('',*,*,#10433,.T.);
#13969=ORIENTED_EDGE('',*,*,#10500,.T.);
#13970=ORIENTED_EDGE('',*,*,#10511,.F.);
#13971=ORIENTED_EDGE('',*,*,#10512,.T.);
#13972=ORIENTED_EDGE('',*,*,#10513,.F.);
#13973=ORIENTED_EDGE('',*,*,#10514,.F.);
#13974=ORIENTED_EDGE('',*,*,#10515,.F.);
#13975=ORIENTED_EDGE('',*,*,#10516,.T.);
#13976=ORIENTED_EDGE('',*,*,#10517,.F.);
#13977=ORIENTED_EDGE('',*,*,#10512,.F.);
#13978=ORIENTED_EDGE('',*,*,#10518,.F.);
#13979=ORIENTED_EDGE('',*,*,#10519,.F.);
#13980=ORIENTED_EDGE('',*,*,#10520,.F.);
#13981=ORIENTED_EDGE('',*,*,#10516,.F.);
#13982=ORIENTED_EDGE('',*,*,#10521,.F.);
#13983=ORIENTED_EDGE('',*,*,#10522,.F.);
#13984=ORIENTED_EDGE('',*,*,#10523,.F.);
#13985=ORIENTED_EDGE('',*,*,#10524,.F.);
#13986=ORIENTED_EDGE('',*,*,#10438,.T.);
#13987=ORIENTED_EDGE('',*,*,#10525,.F.);
#13988=ORIENTED_EDGE('',*,*,#10526,.F.);
#13989=ORIENTED_EDGE('',*,*,#10525,.T.);
#13990=ORIENTED_EDGE('',*,*,#10437,.T.);
#13991=ORIENTED_EDGE('',*,*,#10527,.F.);
#13992=ORIENTED_EDGE('',*,*,#10528,.F.);
#13993=ORIENTED_EDGE('',*,*,#10527,.T.);
#13994=ORIENTED_EDGE('',*,*,#10436,.T.);
#13995=ORIENTED_EDGE('',*,*,#10529,.F.);
#13996=ORIENTED_EDGE('',*,*,#10530,.F.);
#13997=ORIENTED_EDGE('',*,*,#10529,.T.);
#13998=ORIENTED_EDGE('',*,*,#10441,.T.);
#13999=ORIENTED_EDGE('',*,*,#10531,.F.);
#14000=ORIENTED_EDGE('',*,*,#10532,.F.);
#14001=ORIENTED_EDGE('',*,*,#10531,.T.);
#14002=ORIENTED_EDGE('',*,*,#10440,.T.);
#14003=ORIENTED_EDGE('',*,*,#10533,.F.);
#14004=ORIENTED_EDGE('',*,*,#10534,.F.);
#14005=ORIENTED_EDGE('',*,*,#10533,.T.);
#14006=ORIENTED_EDGE('',*,*,#10439,.T.);
#14007=ORIENTED_EDGE('',*,*,#10524,.T.);
#14008=ORIENTED_EDGE('',*,*,#10535,.F.);
#14009=ORIENTED_EDGE('',*,*,#10536,.T.);
#14010=ORIENTED_EDGE('',*,*,#10537,.F.);
#14011=ORIENTED_EDGE('',*,*,#10538,.F.);
#14012=ORIENTED_EDGE('',*,*,#10539,.F.);
#14013=ORIENTED_EDGE('',*,*,#10540,.T.);
#14014=ORIENTED_EDGE('',*,*,#10541,.F.);
#14015=ORIENTED_EDGE('',*,*,#10536,.F.);
#14016=ORIENTED_EDGE('',*,*,#10542,.F.);
#14017=ORIENTED_EDGE('',*,*,#10543,.F.);
#14018=ORIENTED_EDGE('',*,*,#10544,.F.);
#14019=ORIENTED_EDGE('',*,*,#10540,.F.);
#14020=ORIENTED_EDGE('',*,*,#10545,.F.);
#14021=ORIENTED_EDGE('',*,*,#10546,.F.);
#14022=ORIENTED_EDGE('',*,*,#10490,.T.);
#14023=ORIENTED_EDGE('',*,*,#10493,.T.);
#14024=ORIENTED_EDGE('',*,*,#10495,.T.);
#14025=ORIENTED_EDGE('',*,*,#10547,.F.);
#14026=ORIENTED_EDGE('',*,*,#10521,.T.);
#14027=ORIENTED_EDGE('',*,*,#10518,.T.);
#14028=ORIENTED_EDGE('',*,*,#10511,.T.);
#14029=ORIENTED_EDGE('',*,*,#10548,.F.);
#14030=ORIENTED_EDGE('',*,*,#10549,.T.);
#14031=ORIENTED_EDGE('',*,*,#10550,.T.);
#14032=ORIENTED_EDGE('',*,*,#10551,.T.);
#14033=ORIENTED_EDGE('',*,*,#10552,.F.);
#14034=ORIENTED_EDGE('',*,*,#10545,.T.);
#14035=ORIENTED_EDGE('',*,*,#10542,.T.);
#14036=ORIENTED_EDGE('',*,*,#10535,.T.);
#14037=ORIENTED_EDGE('',*,*,#10553,.F.);
#14038=ORIENTED_EDGE('',*,*,#10554,.F.);
#14039=ORIENTED_EDGE('',*,*,#10555,.F.);
#14040=ORIENTED_EDGE('',*,*,#10444,.T.);
#14041=ORIENTED_EDGE('',*,*,#10556,.F.);
#14042=ORIENTED_EDGE('',*,*,#10557,.F.);
#14043=ORIENTED_EDGE('',*,*,#10556,.T.);
#14044=ORIENTED_EDGE('',*,*,#10443,.T.);
#14045=ORIENTED_EDGE('',*,*,#10558,.F.);
#14046=ORIENTED_EDGE('',*,*,#10559,.F.);
#14047=ORIENTED_EDGE('',*,*,#10558,.T.);
#14048=ORIENTED_EDGE('',*,*,#10442,.T.);
#14049=ORIENTED_EDGE('',*,*,#10560,.F.);
#14050=ORIENTED_EDGE('',*,*,#10561,.F.);
#14051=ORIENTED_EDGE('',*,*,#10560,.T.);
#14052=ORIENTED_EDGE('',*,*,#10447,.T.);
#14053=ORIENTED_EDGE('',*,*,#10562,.F.);
#14054=ORIENTED_EDGE('',*,*,#10563,.F.);
#14055=ORIENTED_EDGE('',*,*,#10562,.T.);
#14056=ORIENTED_EDGE('',*,*,#10446,.T.);
#14057=ORIENTED_EDGE('',*,*,#10564,.F.);
#14058=ORIENTED_EDGE('',*,*,#10565,.F.);
#14059=ORIENTED_EDGE('',*,*,#10564,.T.);
#14060=ORIENTED_EDGE('',*,*,#10445,.T.);
#14061=ORIENTED_EDGE('',*,*,#10555,.T.);
#14062=ORIENTED_EDGE('',*,*,#10551,.F.);
#14063=ORIENTED_EDGE('',*,*,#10566,.T.);
#14064=ORIENTED_EDGE('',*,*,#10567,.F.);
#14065=ORIENTED_EDGE('',*,*,#10568,.F.);
#14066=ORIENTED_EDGE('',*,*,#10569,.F.);
#14067=ORIENTED_EDGE('',*,*,#10570,.T.);
#14068=ORIENTED_EDGE('',*,*,#10571,.F.);
#14069=ORIENTED_EDGE('',*,*,#10566,.F.);
#14070=ORIENTED_EDGE('',*,*,#10550,.F.);
#14071=ORIENTED_EDGE('',*,*,#10572,.F.);
#14072=ORIENTED_EDGE('',*,*,#10573,.F.);
#14073=ORIENTED_EDGE('',*,*,#10570,.F.);
#14074=ORIENTED_EDGE('',*,*,#10549,.F.);
#14075=ORIENTED_EDGE('',*,*,#10574,.F.);
#14076=ORIENTED_EDGE('',*,*,#10575,.T.);
#14077=ORIENTED_EDGE('',*,*,#10450,.F.);
#14078=ORIENTED_EDGE('',*,*,#10576,.T.);
#14079=ORIENTED_EDGE('',*,*,#10577,.F.);
#14080=ORIENTED_EDGE('',*,*,#10576,.F.);
#14081=ORIENTED_EDGE('',*,*,#10449,.F.);
#14082=ORIENTED_EDGE('',*,*,#10578,.T.);
#14083=ORIENTED_EDGE('',*,*,#10579,.F.);
#14084=ORIENTED_EDGE('',*,*,#10578,.F.);
#14085=ORIENTED_EDGE('',*,*,#10448,.F.);
#14086=ORIENTED_EDGE('',*,*,#10580,.T.);
#14087=ORIENTED_EDGE('',*,*,#10581,.F.);
#14088=ORIENTED_EDGE('',*,*,#10580,.F.);
#14089=ORIENTED_EDGE('',*,*,#10462,.F.);
#14090=ORIENTED_EDGE('',*,*,#10582,.T.);
#14091=ORIENTED_EDGE('',*,*,#10583,.F.);
#14092=ORIENTED_EDGE('',*,*,#10582,.F.);
#14093=ORIENTED_EDGE('',*,*,#10461,.F.);
#14094=ORIENTED_EDGE('',*,*,#10584,.T.);
#14095=ORIENTED_EDGE('',*,*,#10585,.F.);
#14096=ORIENTED_EDGE('',*,*,#10584,.F.);
#14097=ORIENTED_EDGE('',*,*,#10460,.F.);
#14098=ORIENTED_EDGE('',*,*,#10586,.T.);
#14099=ORIENTED_EDGE('',*,*,#10587,.F.);
#14100=ORIENTED_EDGE('',*,*,#10586,.F.);
#14101=ORIENTED_EDGE('',*,*,#10459,.F.);
#14102=ORIENTED_EDGE('',*,*,#10588,.T.);
#14103=ORIENTED_EDGE('',*,*,#10589,.F.);
#14104=ORIENTED_EDGE('',*,*,#10458,.F.);
#14105=ORIENTED_EDGE('',*,*,#10590,.T.);
#14106=ORIENTED_EDGE('',*,*,#10591,.F.);
#14107=ORIENTED_EDGE('',*,*,#10588,.F.);
#14108=ORIENTED_EDGE('',*,*,#10590,.F.);
#14109=ORIENTED_EDGE('',*,*,#10457,.F.);
#14110=ORIENTED_EDGE('',*,*,#10592,.T.);
#14111=ORIENTED_EDGE('',*,*,#10593,.F.);
#14112=ORIENTED_EDGE('',*,*,#10592,.F.);
#14113=ORIENTED_EDGE('',*,*,#10456,.F.);
#14114=ORIENTED_EDGE('',*,*,#10594,.T.);
#14115=ORIENTED_EDGE('',*,*,#10595,.F.);
#14116=ORIENTED_EDGE('',*,*,#10594,.F.);
#14117=ORIENTED_EDGE('',*,*,#10455,.F.);
#14118=ORIENTED_EDGE('',*,*,#10391,.T.);
#14119=ORIENTED_EDGE('',*,*,#10596,.F.);
#14120=ORIENTED_EDGE('',*,*,#10389,.F.);
#14121=ORIENTED_EDGE('',*,*,#10454,.F.);
#14122=ORIENTED_EDGE('',*,*,#10597,.T.);
#14123=ORIENTED_EDGE('',*,*,#10598,.F.);
#14124=ORIENTED_EDGE('',*,*,#10597,.F.);
#14125=ORIENTED_EDGE('',*,*,#10453,.F.);
#14126=ORIENTED_EDGE('',*,*,#10599,.T.);
#14127=ORIENTED_EDGE('',*,*,#10600,.F.);
#14128=ORIENTED_EDGE('',*,*,#10599,.F.);
#14129=ORIENTED_EDGE('',*,*,#10452,.F.);
#14130=ORIENTED_EDGE('',*,*,#10601,.T.);
#14131=ORIENTED_EDGE('',*,*,#10602,.F.);
#14132=ORIENTED_EDGE('',*,*,#10451,.F.);
#14133=ORIENTED_EDGE('',*,*,#10575,.F.);
#14134=ORIENTED_EDGE('',*,*,#10603,.F.);
#14135=ORIENTED_EDGE('',*,*,#10601,.F.);
#14136=ORIENTED_EDGE('',*,*,#10604,.T.);
#14137=ORIENTED_EDGE('',*,*,#10464,.F.);
#14138=ORIENTED_EDGE('',*,*,#10605,.T.);
#14139=ORIENTED_EDGE('',*,*,#10606,.F.);
#14140=ORIENTED_EDGE('',*,*,#10605,.F.);
#14141=ORIENTED_EDGE('',*,*,#10463,.F.);
#14142=ORIENTED_EDGE('',*,*,#10607,.T.);
#14143=ORIENTED_EDGE('',*,*,#10608,.F.);
#14144=ORIENTED_EDGE('',*,*,#10607,.F.);
#14145=ORIENTED_EDGE('',*,*,#10468,.F.);
#14146=ORIENTED_EDGE('',*,*,#10609,.T.);
#14147=ORIENTED_EDGE('',*,*,#10610,.F.);
#14148=ORIENTED_EDGE('',*,*,#10609,.F.);
#14149=ORIENTED_EDGE('',*,*,#10467,.F.);
#14150=ORIENTED_EDGE('',*,*,#10611,.T.);
#14151=ORIENTED_EDGE('',*,*,#10612,.F.);
#14152=ORIENTED_EDGE('',*,*,#10611,.F.);
#14153=ORIENTED_EDGE('',*,*,#10466,.F.);
#14154=ORIENTED_EDGE('',*,*,#10613,.T.);
#14155=ORIENTED_EDGE('',*,*,#10614,.F.);
#14156=ORIENTED_EDGE('',*,*,#10613,.F.);
#14157=ORIENTED_EDGE('',*,*,#10465,.F.);
#14158=ORIENTED_EDGE('',*,*,#10604,.F.);
#14159=ORIENTED_EDGE('',*,*,#10615,.F.);
#14160=ORIENTED_EDGE('',*,*,#10616,.T.);
#14161=ORIENTED_EDGE('',*,*,#10470,.F.);
#14162=ORIENTED_EDGE('',*,*,#10617,.T.);
#14163=ORIENTED_EDGE('',*,*,#10618,.F.);
#14164=ORIENTED_EDGE('',*,*,#10617,.F.);
#14165=ORIENTED_EDGE('',*,*,#10469,.F.);
#14166=ORIENTED_EDGE('',*,*,#10619,.T.);
#14167=ORIENTED_EDGE('',*,*,#10620,.F.);
#14168=ORIENTED_EDGE('',*,*,#10619,.F.);
#14169=ORIENTED_EDGE('',*,*,#10474,.F.);
#14170=ORIENTED_EDGE('',*,*,#10621,.T.);
#14171=ORIENTED_EDGE('',*,*,#10622,.F.);
#14172=ORIENTED_EDGE('',*,*,#10621,.F.);
#14173=ORIENTED_EDGE('',*,*,#10473,.F.);
#14174=ORIENTED_EDGE('',*,*,#10623,.T.);
#14175=ORIENTED_EDGE('',*,*,#10624,.F.);
#14176=ORIENTED_EDGE('',*,*,#10623,.F.);
#14177=ORIENTED_EDGE('',*,*,#10472,.F.);
#14178=ORIENTED_EDGE('',*,*,#10625,.T.);
#14179=ORIENTED_EDGE('',*,*,#10626,.F.);
#14180=ORIENTED_EDGE('',*,*,#10625,.F.);
#14181=ORIENTED_EDGE('',*,*,#10471,.F.);
#14182=ORIENTED_EDGE('',*,*,#10616,.F.);
#14183=ORIENTED_EDGE('',*,*,#10627,.F.);
#14184=ORIENTED_EDGE('',*,*,#10539,.T.);
#14185=ORIENTED_EDGE('',*,*,#10628,.F.);
#14186=ORIENTED_EDGE('',*,*,#10491,.T.);
#14187=ORIENTED_EDGE('',*,*,#10553,.T.);
#14188=ORIENTED_EDGE('',*,*,#10522,.T.);
#14189=ORIENTED_EDGE('',*,*,#10547,.T.);
#14190=ORIENTED_EDGE('',*,*,#10498,.T.);
#14191=ORIENTED_EDGE('',*,*,#10629,.F.);
#14192=ORIENTED_EDGE('',*,*,#10630,.F.);
#14193=ORIENTED_EDGE('',*,*,#10631,.F.);
#14194=ORIENTED_EDGE('',*,*,#10496,.F.);
#14195=ORIENTED_EDGE('',*,*,#10494,.F.);
#14196=ORIENTED_EDGE('',*,*,#10488,.F.);
#14197=ORIENTED_EDGE('',*,*,#10632,.F.);
#14198=ORIENTED_EDGE('',*,*,#10484,.F.);
#14199=ORIENTED_EDGE('',*,*,#10482,.F.);
#14200=ORIENTED_EDGE('',*,*,#10480,.F.);
#14201=ORIENTED_EDGE('',*,*,#10478,.F.);
#14202=ORIENTED_EDGE('',*,*,#10475,.F.);
#14203=ORIENTED_EDGE('',*,*,#10486,.F.);
#14204=ORIENTED_EDGE('',*,*,#10515,.T.);
#14205=ORIENTED_EDGE('',*,*,#10633,.F.);
#14206=ORIENTED_EDGE('',*,*,#10574,.T.);
#14207=ORIENTED_EDGE('',*,*,#10548,.T.);
#14208=ORIENTED_EDGE('',*,*,#10517,.T.);
#14209=ORIENTED_EDGE('',*,*,#10520,.T.);
#14210=ORIENTED_EDGE('',*,*,#10634,.F.);
#14211=ORIENTED_EDGE('',*,*,#10635,.F.);
#14212=ORIENTED_EDGE('',*,*,#10636,.F.);
#14213=ORIENTED_EDGE('',*,*,#10513,.T.);
#14214=ORIENTED_EDGE('',*,*,#10508,.T.);
#14215=ORIENTED_EDGE('',*,*,#10510,.T.);
#14216=ORIENTED_EDGE('',*,*,#10499,.T.);
#14217=ORIENTED_EDGE('',*,*,#10502,.T.);
#14218=ORIENTED_EDGE('',*,*,#10504,.T.);
#14219=ORIENTED_EDGE('',*,*,#10506,.T.);
#14220=ORIENTED_EDGE('',*,*,#10541,.T.);
#14221=ORIENTED_EDGE('',*,*,#10544,.T.);
#14222=ORIENTED_EDGE('',*,*,#10637,.F.);
#14223=ORIENTED_EDGE('',*,*,#10638,.F.);
#14224=ORIENTED_EDGE('',*,*,#10639,.F.);
#14225=ORIENTED_EDGE('',*,*,#10537,.T.);
#14226=ORIENTED_EDGE('',*,*,#10532,.T.);
#14227=ORIENTED_EDGE('',*,*,#10534,.T.);
#14228=ORIENTED_EDGE('',*,*,#10523,.T.);
#14229=ORIENTED_EDGE('',*,*,#10526,.T.);
#14230=ORIENTED_EDGE('',*,*,#10528,.T.);
#14231=ORIENTED_EDGE('',*,*,#10530,.T.);
#14232=ORIENTED_EDGE('',*,*,#10569,.T.);
#14233=ORIENTED_EDGE('',*,*,#10640,.F.);
#14234=ORIENTED_EDGE('',*,*,#10546,.T.);
#14235=ORIENTED_EDGE('',*,*,#10552,.T.);
#14236=ORIENTED_EDGE('',*,*,#10571,.T.);
#14237=ORIENTED_EDGE('',*,*,#10573,.T.);
#14238=ORIENTED_EDGE('',*,*,#10641,.F.);
#14239=ORIENTED_EDGE('',*,*,#10642,.F.);
#14240=ORIENTED_EDGE('',*,*,#10643,.F.);
#14241=ORIENTED_EDGE('',*,*,#10567,.T.);
#14242=ORIENTED_EDGE('',*,*,#10563,.T.);
#14243=ORIENTED_EDGE('',*,*,#10565,.T.);
#14244=ORIENTED_EDGE('',*,*,#10554,.T.);
#14245=ORIENTED_EDGE('',*,*,#10557,.T.);
#14246=ORIENTED_EDGE('',*,*,#10559,.T.);
#14247=ORIENTED_EDGE('',*,*,#10561,.T.);
#14248=ORIENTED_EDGE('',*,*,#10644,.F.);
#14249=ORIENTED_EDGE('',*,*,#10645,.F.);
#14250=ORIENTED_EDGE('',*,*,#10646,.F.);
#14251=ORIENTED_EDGE('',*,*,#10647,.F.);
#14252=ORIENTED_EDGE('',*,*,#10646,.T.);
#14253=ORIENTED_EDGE('',*,*,#10648,.F.);
#14254=ORIENTED_EDGE('',*,*,#10649,.F.);
#14255=ORIENTED_EDGE('',*,*,#10650,.F.);
#14256=ORIENTED_EDGE('',*,*,#10649,.T.);
#14257=ORIENTED_EDGE('',*,*,#10651,.F.);
#14258=ORIENTED_EDGE('',*,*,#10652,.F.);
#14259=ORIENTED_EDGE('',*,*,#10653,.F.);
#14260=ORIENTED_EDGE('',*,*,#10419,.F.);
#14261=ORIENTED_EDGE('',*,*,#10654,.F.);
#14262=ORIENTED_EDGE('',*,*,#10655,.F.);
#14263=ORIENTED_EDGE('',*,*,#10656,.F.);
#14264=ORIENTED_EDGE('',*,*,#10655,.T.);
#14265=ORIENTED_EDGE('',*,*,#10657,.F.);
#14266=ORIENTED_EDGE('',*,*,#10658,.F.);
#14267=ORIENTED_EDGE('',*,*,#10659,.F.);
#14268=ORIENTED_EDGE('',*,*,#10660,.F.);
#14269=ORIENTED_EDGE('',*,*,#10658,.T.);
#14270=ORIENTED_EDGE('',*,*,#10661,.F.);
#14271=ORIENTED_EDGE('',*,*,#10412,.F.);
#14272=ORIENTED_EDGE('',*,*,#10399,.F.);
#14273=ORIENTED_EDGE('',*,*,#10662,.F.);
#14274=ORIENTED_EDGE('',*,*,#10663,.F.);
#14275=ORIENTED_EDGE('',*,*,#10128,.F.);
#14276=ORIENTED_EDGE('',*,*,#10663,.T.);
#14277=ORIENTED_EDGE('',*,*,#10664,.F.);
#14278=ORIENTED_EDGE('',*,*,#10665,.F.);
#14279=ORIENTED_EDGE('',*,*,#10129,.F.);
#14280=ORIENTED_EDGE('',*,*,#10130,.F.);
#14281=ORIENTED_EDGE('',*,*,#10665,.T.);
#14282=ORIENTED_EDGE('',*,*,#10666,.F.);
#14283=ORIENTED_EDGE('',*,*,#10123,.F.);
#14284=ORIENTED_EDGE('',*,*,#10667,.T.);
#14285=ORIENTED_EDGE('',*,*,#10668,.F.);
#14286=ORIENTED_EDGE('',*,*,#10669,.F.);
#14287=ORIENTED_EDGE('',*,*,#10670,.F.);
#14288=ORIENTED_EDGE('',*,*,#10669,.T.);
#14289=ORIENTED_EDGE('',*,*,#10671,.F.);
#14290=ORIENTED_EDGE('',*,*,#10672,.F.);
#14291=ORIENTED_EDGE('',*,*,#10673,.F.);
#14292=ORIENTED_EDGE('',*,*,#10674,.F.);
#14293=ORIENTED_EDGE('',*,*,#10672,.T.);
#14294=ORIENTED_EDGE('',*,*,#10675,.F.);
#14295=ORIENTED_EDGE('',*,*,#10676,.F.);
#14296=ORIENTED_EDGE('',*,*,#10677,.T.);
#14297=ORIENTED_EDGE('',*,*,#10678,.F.);
#14298=ORIENTED_EDGE('',*,*,#10124,.F.);
#14299=ORIENTED_EDGE('',*,*,#10666,.T.);
#14300=ORIENTED_EDGE('',*,*,#10664,.T.);
#14301=ORIENTED_EDGE('',*,*,#10662,.T.);
#14302=ORIENTED_EDGE('',*,*,#10679,.F.);
#14303=ORIENTED_EDGE('',*,*,#10680,.F.);
#14304=ORIENTED_EDGE('',*,*,#10681,.T.);
#14305=ORIENTED_EDGE('',*,*,#10682,.T.);
#14306=ORIENTED_EDGE('',*,*,#10683,.T.);
#14307=ORIENTED_EDGE('',*,*,#10684,.T.);
#14308=ORIENTED_EDGE('',*,*,#10685,.T.);
#14309=ORIENTED_EDGE('',*,*,#10686,.T.);
#14310=ORIENTED_EDGE('',*,*,#10404,.T.);
#14311=ORIENTED_EDGE('',*,*,#10687,.F.);
#14312=ORIENTED_EDGE('',*,*,#10688,.F.);
#14313=ORIENTED_EDGE('',*,*,#10661,.T.);
#14314=ORIENTED_EDGE('',*,*,#10657,.T.);
#14315=ORIENTED_EDGE('',*,*,#10654,.T.);
#14316=ORIENTED_EDGE('',*,*,#10689,.F.);
#14317=ORIENTED_EDGE('',*,*,#10690,.F.);
#14318=ORIENTED_EDGE('',*,*,#10691,.T.);
#14319=ORIENTED_EDGE('',*,*,#10692,.T.);
#14320=ORIENTED_EDGE('',*,*,#10693,.T.);
#14321=ORIENTED_EDGE('',*,*,#10694,.T.);
#14322=ORIENTED_EDGE('',*,*,#10695,.T.);
#14323=ORIENTED_EDGE('',*,*,#10696,.T.);
#14324=ORIENTED_EDGE('',*,*,#10697,.T.);
#14325=ORIENTED_EDGE('',*,*,#10698,.F.);
#14326=ORIENTED_EDGE('',*,*,#10699,.F.);
#14327=ORIENTED_EDGE('',*,*,#10651,.T.);
#14328=ORIENTED_EDGE('',*,*,#10648,.T.);
#14329=ORIENTED_EDGE('',*,*,#10645,.T.);
#14330=ORIENTED_EDGE('',*,*,#10700,.F.);
#14331=ORIENTED_EDGE('',*,*,#10701,.F.);
#14332=ORIENTED_EDGE('',*,*,#10702,.T.);
#14333=ORIENTED_EDGE('',*,*,#10703,.T.);
#14334=ORIENTED_EDGE('',*,*,#10704,.T.);
#14335=ORIENTED_EDGE('',*,*,#10705,.T.);
#14336=ORIENTED_EDGE('',*,*,#10706,.T.);
#14337=ORIENTED_EDGE('',*,*,#10707,.T.);
#14338=ORIENTED_EDGE('',*,*,#10708,.T.);
#14339=ORIENTED_EDGE('',*,*,#10709,.F.);
#14340=ORIENTED_EDGE('',*,*,#10710,.F.);
#14341=ORIENTED_EDGE('',*,*,#10675,.T.);
#14342=ORIENTED_EDGE('',*,*,#10671,.T.);
#14343=ORIENTED_EDGE('',*,*,#10668,.T.);
#14344=ORIENTED_EDGE('',*,*,#10711,.T.);
#14345=ORIENTED_EDGE('',*,*,#10712,.F.);
#14346=ORIENTED_EDGE('',*,*,#10713,.T.);
#14347=ORIENTED_EDGE('',*,*,#10714,.T.);
#14348=ORIENTED_EDGE('',*,*,#10715,.T.);
#14349=ORIENTED_EDGE('',*,*,#10716,.T.);
#14350=ORIENTED_EDGE('',*,*,#10717,.T.);
#14351=ORIENTED_EDGE('',*,*,#10718,.T.);
#14352=ORIENTED_EDGE('',*,*,#10603,.T.);
#14353=ORIENTED_EDGE('',*,*,#10577,.T.);
#14354=ORIENTED_EDGE('',*,*,#10579,.T.);
#14355=ORIENTED_EDGE('',*,*,#10581,.T.);
#14356=ORIENTED_EDGE('',*,*,#10583,.T.);
#14357=ORIENTED_EDGE('',*,*,#10585,.T.);
#14358=ORIENTED_EDGE('',*,*,#10587,.T.);
#14359=ORIENTED_EDGE('',*,*,#10589,.T.);
#14360=ORIENTED_EDGE('',*,*,#10591,.T.);
#14361=ORIENTED_EDGE('',*,*,#10593,.T.);
#14362=ORIENTED_EDGE('',*,*,#10595,.T.);
#14363=ORIENTED_EDGE('',*,*,#10596,.T.);
#14364=ORIENTED_EDGE('',*,*,#10390,.T.);
#14365=ORIENTED_EDGE('',*,*,#10598,.T.);
#14366=ORIENTED_EDGE('',*,*,#10600,.T.);
#14367=ORIENTED_EDGE('',*,*,#10602,.T.);
#14368=ORIENTED_EDGE('',*,*,#10383,.T.);
#14369=ORIENTED_EDGE('',*,*,#10384,.F.);
#14370=ORIENTED_EDGE('',*,*,#10379,.F.);
#14371=ORIENTED_EDGE('',*,*,#10614,.T.);
#14372=ORIENTED_EDGE('',*,*,#10615,.T.);
#14373=ORIENTED_EDGE('',*,*,#10606,.T.);
#14374=ORIENTED_EDGE('',*,*,#10608,.T.);
#14375=ORIENTED_EDGE('',*,*,#10610,.T.);
#14376=ORIENTED_EDGE('',*,*,#10612,.T.);
#14377=ORIENTED_EDGE('',*,*,#10376,.F.);
#14378=ORIENTED_EDGE('',*,*,#10626,.T.);
#14379=ORIENTED_EDGE('',*,*,#10627,.T.);
#14380=ORIENTED_EDGE('',*,*,#10618,.T.);
#14381=ORIENTED_EDGE('',*,*,#10620,.T.);
#14382=ORIENTED_EDGE('',*,*,#10622,.T.);
#14383=ORIENTED_EDGE('',*,*,#10624,.T.);
#14384=ORIENTED_EDGE('',*,*,#10719,.T.);
#14385=ORIENTED_EDGE('',*,*,#10720,.F.);
#14386=ORIENTED_EDGE('',*,*,#10638,.T.);
#14387=ORIENTED_EDGE('',*,*,#10721,.F.);
#14388=ORIENTED_EDGE('',*,*,#10722,.T.);
#14389=ORIENTED_EDGE('',*,*,#10723,.F.);
#14390=ORIENTED_EDGE('',*,*,#10632,.T.);
#14391=ORIENTED_EDGE('',*,*,#10487,.T.);
#14392=ORIENTED_EDGE('',*,*,#10628,.T.);
#14393=ORIENTED_EDGE('',*,*,#10538,.T.);
#14394=ORIENTED_EDGE('',*,*,#10639,.T.);
#14395=ORIENTED_EDGE('',*,*,#10720,.T.);
#14396=ORIENTED_EDGE('',*,*,#10724,.T.);
#14397=ORIENTED_EDGE('',*,*,#10725,.F.);
#14398=ORIENTED_EDGE('',*,*,#10630,.T.);
#14399=ORIENTED_EDGE('',*,*,#10723,.T.);
#14400=ORIENTED_EDGE('',*,*,#10726,.T.);
#14401=ORIENTED_EDGE('',*,*,#10727,.F.);
#14402=ORIENTED_EDGE('',*,*,#10634,.T.);
#14403=ORIENTED_EDGE('',*,*,#10519,.T.);
#14404=ORIENTED_EDGE('',*,*,#10629,.T.);
#14405=ORIENTED_EDGE('',*,*,#10497,.T.);
#14406=ORIENTED_EDGE('',*,*,#10631,.T.);
#14407=ORIENTED_EDGE('',*,*,#10725,.T.);
#14408=ORIENTED_EDGE('',*,*,#10728,.T.);
#14409=ORIENTED_EDGE('',*,*,#10729,.F.);
#14410=ORIENTED_EDGE('',*,*,#10635,.T.);
#14411=ORIENTED_EDGE('',*,*,#10727,.T.);
#14412=ORIENTED_EDGE('',*,*,#10730,.T.);
#14413=ORIENTED_EDGE('',*,*,#10731,.F.);
#14414=ORIENTED_EDGE('',*,*,#10641,.T.);
#14415=ORIENTED_EDGE('',*,*,#10572,.T.);
#14416=ORIENTED_EDGE('',*,*,#10633,.T.);
#14417=ORIENTED_EDGE('',*,*,#10514,.T.);
#14418=ORIENTED_EDGE('',*,*,#10636,.T.);
#14419=ORIENTED_EDGE('',*,*,#10729,.T.);
#14420=ORIENTED_EDGE('',*,*,#10732,.T.);
#14421=ORIENTED_EDGE('',*,*,#10733,.F.);
#14422=ORIENTED_EDGE('',*,*,#10642,.T.);
#14423=ORIENTED_EDGE('',*,*,#10731,.T.);
#14424=ORIENTED_EDGE('',*,*,#10734,.T.);
#14425=ORIENTED_EDGE('',*,*,#10721,.T.);
#14426=ORIENTED_EDGE('',*,*,#10637,.T.);
#14427=ORIENTED_EDGE('',*,*,#10543,.T.);
#14428=ORIENTED_EDGE('',*,*,#10640,.T.);
#14429=ORIENTED_EDGE('',*,*,#10568,.T.);
#14430=ORIENTED_EDGE('',*,*,#10643,.T.);
#14431=ORIENTED_EDGE('',*,*,#10733,.T.);
#14432=ORIENTED_EDGE('',*,*,#10735,.F.);
#14433=ORIENTED_EDGE('',*,*,#10422,.T.);
#14434=ORIENTED_EDGE('',*,*,#10736,.F.);
#14435=ORIENTED_EDGE('',*,*,#10700,.T.);
#14436=ORIENTED_EDGE('',*,*,#10644,.T.);
#14437=ORIENTED_EDGE('',*,*,#10647,.T.);
#14438=ORIENTED_EDGE('',*,*,#10650,.T.);
#14439=ORIENTED_EDGE('',*,*,#10653,.T.);
#14440=ORIENTED_EDGE('',*,*,#10737,.F.);
#14441=ORIENTED_EDGE('',*,*,#10738,.F.);
#14442=ORIENTED_EDGE('',*,*,#10735,.T.);
#14443=ORIENTED_EDGE('',*,*,#10739,.F.);
#14444=ORIENTED_EDGE('',*,*,#10420,.T.);
#14445=ORIENTED_EDGE('',*,*,#10737,.T.);
#14446=ORIENTED_EDGE('',*,*,#10652,.T.);
#14447=ORIENTED_EDGE('',*,*,#10699,.T.);
#14448=ORIENTED_EDGE('',*,*,#10739,.T.);
#14449=ORIENTED_EDGE('',*,*,#10698,.T.);
#14450=ORIENTED_EDGE('',*,*,#10740,.T.);
#14451=ORIENTED_EDGE('',*,*,#10741,.F.);
#14452=ORIENTED_EDGE('',*,*,#10742,.F.);
#14453=ORIENTED_EDGE('',*,*,#10743,.T.);
#14454=ORIENTED_EDGE('',*,*,#10744,.F.);
#14455=ORIENTED_EDGE('',*,*,#10740,.F.);
#14456=ORIENTED_EDGE('',*,*,#10697,.F.);
#14457=ORIENTED_EDGE('',*,*,#10745,.T.);
#14458=ORIENTED_EDGE('',*,*,#10746,.F.);
#14459=ORIENTED_EDGE('',*,*,#10743,.F.);
#14460=ORIENTED_EDGE('',*,*,#10696,.F.);
#14461=ORIENTED_EDGE('',*,*,#10747,.T.);
#14462=ORIENTED_EDGE('',*,*,#10748,.F.);
#14463=ORIENTED_EDGE('',*,*,#10745,.F.);
#14464=ORIENTED_EDGE('',*,*,#10749,.F.);
#14465=ORIENTED_EDGE('',*,*,#10750,.T.);
#14466=ORIENTED_EDGE('',*,*,#10695,.F.);
#14467=ORIENTED_EDGE('',*,*,#10751,.T.);
#14468=ORIENTED_EDGE('',*,*,#10752,.F.);
#14469=ORIENTED_EDGE('',*,*,#10750,.F.);
#14470=ORIENTED_EDGE('',*,*,#10753,.F.);
#14471=ORIENTED_EDGE('',*,*,#10747,.F.);
#14472=ORIENTED_EDGE('',*,*,#10694,.F.);
#14473=ORIENTED_EDGE('',*,*,#10754,.T.);
#14474=ORIENTED_EDGE('',*,*,#10755,.F.);
#14475=ORIENTED_EDGE('',*,*,#10751,.F.);
#14476=ORIENTED_EDGE('',*,*,#10756,.F.);
#14477=ORIENTED_EDGE('',*,*,#10757,.T.);
#14478=ORIENTED_EDGE('',*,*,#10693,.F.);
#14479=ORIENTED_EDGE('',*,*,#10758,.T.);
#14480=ORIENTED_EDGE('',*,*,#10759,.F.);
#14481=ORIENTED_EDGE('',*,*,#10757,.F.);
#14482=ORIENTED_EDGE('',*,*,#10760,.F.);
#14483=ORIENTED_EDGE('',*,*,#10754,.F.);
#14484=ORIENTED_EDGE('',*,*,#10692,.F.);
#14485=ORIENTED_EDGE('',*,*,#10761,.T.);
#14486=ORIENTED_EDGE('',*,*,#10762,.F.);
#14487=ORIENTED_EDGE('',*,*,#10758,.F.);
#14488=ORIENTED_EDGE('',*,*,#10763,.F.);
#14489=ORIENTED_EDGE('',*,*,#10764,.T.);
#14490=ORIENTED_EDGE('',*,*,#10691,.F.);
#14491=ORIENTED_EDGE('',*,*,#10765,.F.);
#14492=ORIENTED_EDGE('',*,*,#10766,.F.);
#14493=ORIENTED_EDGE('',*,*,#10764,.F.);
#14494=ORIENTED_EDGE('',*,*,#10767,.F.);
#14495=ORIENTED_EDGE('',*,*,#10761,.F.);
#14496=ORIENTED_EDGE('',*,*,#10417,.F.);
#14497=ORIENTED_EDGE('',*,*,#10768,.F.);
#14498=ORIENTED_EDGE('',*,*,#10765,.T.);
#14499=ORIENTED_EDGE('',*,*,#10690,.T.);
#14500=ORIENTED_EDGE('',*,*,#10689,.T.);
#14501=ORIENTED_EDGE('',*,*,#10418,.T.);
#14502=ORIENTED_EDGE('',*,*,#10656,.T.);
#14503=ORIENTED_EDGE('',*,*,#10659,.T.);
#14504=ORIENTED_EDGE('',*,*,#10660,.T.);
#14505=ORIENTED_EDGE('',*,*,#10411,.F.);
#14506=ORIENTED_EDGE('',*,*,#10769,.F.);
#14507=ORIENTED_EDGE('',*,*,#10416,.T.);
#14508=ORIENTED_EDGE('',*,*,#10688,.T.);
#14509=ORIENTED_EDGE('',*,*,#10413,.T.);
#14510=ORIENTED_EDGE('',*,*,#10362,.F.);
#14511=ORIENTED_EDGE('',*,*,#10770,.T.);
#14512=ORIENTED_EDGE('',*,*,#10397,.F.);
#14513=ORIENTED_EDGE('',*,*,#10364,.F.);
#14514=ORIENTED_EDGE('',*,*,#10771,.T.);
#14515=ORIENTED_EDGE('',*,*,#10401,.T.);
#14516=ORIENTED_EDGE('',*,*,#10772,.T.);
#14517=ORIENTED_EDGE('',*,*,#10680,.T.);
#14518=ORIENTED_EDGE('',*,*,#10410,.T.);
#14519=ORIENTED_EDGE('',*,*,#10687,.T.);
#14520=ORIENTED_EDGE('',*,*,#10403,.T.);
#14521=ORIENTED_EDGE('',*,*,#10773,.T.);
#14522=ORIENTED_EDGE('',*,*,#10407,.T.);
#14523=ORIENTED_EDGE('',*,*,#10368,.F.);
#14524=ORIENTED_EDGE('',*,*,#10370,.F.);
#14525=ORIENTED_EDGE('',*,*,#10406,.T.);
#14526=ORIENTED_EDGE('',*,*,#10773,.F.);
#14527=ORIENTED_EDGE('',*,*,#10402,.T.);
#14528=ORIENTED_EDGE('',*,*,#10686,.F.);
#14529=ORIENTED_EDGE('',*,*,#10774,.T.);
#14530=ORIENTED_EDGE('',*,*,#10372,.F.);
#14531=ORIENTED_EDGE('',*,*,#10405,.F.);
#14532=ORIENTED_EDGE('',*,*,#10374,.F.);
#14533=ORIENTED_EDGE('',*,*,#10775,.T.);
#14534=ORIENTED_EDGE('',*,*,#10685,.F.);
#14535=ORIENTED_EDGE('',*,*,#10776,.T.);
#14536=ORIENTED_EDGE('',*,*,#10375,.F.);
#14537=ORIENTED_EDGE('',*,*,#10775,.F.);
#14538=ORIENTED_EDGE('',*,*,#10373,.F.);
#14539=ORIENTED_EDGE('',*,*,#10774,.F.);
#14540=ORIENTED_EDGE('',*,*,#10684,.F.);
#14541=ORIENTED_EDGE('',*,*,#10777,.T.);
#14542=ORIENTED_EDGE('',*,*,#10356,.F.);
#14543=ORIENTED_EDGE('',*,*,#10776,.F.);
#14544=ORIENTED_EDGE('',*,*,#10358,.F.);
#14545=ORIENTED_EDGE('',*,*,#10778,.T.);
#14546=ORIENTED_EDGE('',*,*,#10683,.F.);
#14547=ORIENTED_EDGE('',*,*,#10779,.T.);
#14548=ORIENTED_EDGE('',*,*,#10359,.F.);
#14549=ORIENTED_EDGE('',*,*,#10778,.F.);
#14550=ORIENTED_EDGE('',*,*,#10357,.F.);
#14551=ORIENTED_EDGE('',*,*,#10777,.F.);
#14552=ORIENTED_EDGE('',*,*,#10682,.F.);
#14553=ORIENTED_EDGE('',*,*,#10780,.T.);
#14554=ORIENTED_EDGE('',*,*,#10360,.F.);
#14555=ORIENTED_EDGE('',*,*,#10779,.F.);
#14556=ORIENTED_EDGE('',*,*,#10772,.F.);
#14557=ORIENTED_EDGE('',*,*,#10400,.T.);
#14558=ORIENTED_EDGE('',*,*,#10771,.F.);
#14559=ORIENTED_EDGE('',*,*,#10363,.F.);
#14560=ORIENTED_EDGE('',*,*,#10770,.F.);
#14561=ORIENTED_EDGE('',*,*,#10361,.F.);
#14562=ORIENTED_EDGE('',*,*,#10780,.F.);
#14563=ORIENTED_EDGE('',*,*,#10681,.F.);
#14564=ORIENTED_EDGE('',*,*,#10679,.T.);
#14565=ORIENTED_EDGE('',*,*,#10398,.T.);
#14566=ORIENTED_EDGE('',*,*,#10126,.T.);
#14567=ORIENTED_EDGE('',*,*,#10781,.F.);
#14568=ORIENTED_EDGE('',*,*,#10121,.T.);
#14569=ORIENTED_EDGE('',*,*,#10782,.F.);
#14570=ORIENTED_EDGE('',*,*,#10125,.T.);
#14571=ORIENTED_EDGE('',*,*,#10678,.T.);
#14572=ORIENTED_EDGE('',*,*,#10783,.T.);
#14573=ORIENTED_EDGE('',*,*,#10784,.F.);
#14574=ORIENTED_EDGE('',*,*,#10785,.F.);
#14575=ORIENTED_EDGE('',*,*,#10786,.T.);
#14576=ORIENTED_EDGE('',*,*,#10786,.F.);
#14577=ORIENTED_EDGE('',*,*,#10787,.F.);
#14578=ORIENTED_EDGE('',*,*,#10783,.F.);
#14579=ORIENTED_EDGE('',*,*,#10677,.F.);
#14580=ORIENTED_EDGE('',*,*,#10788,.T.);
#14581=ORIENTED_EDGE('',*,*,#10789,.F.);
#14582=ORIENTED_EDGE('',*,*,#10718,.F.);
#14583=ORIENTED_EDGE('',*,*,#10790,.T.);
#14584=ORIENTED_EDGE('',*,*,#10791,.F.);
#14585=ORIENTED_EDGE('',*,*,#10788,.F.);
#14586=ORIENTED_EDGE('',*,*,#10792,.F.);
#14587=ORIENTED_EDGE('',*,*,#10793,.T.);
#14588=ORIENTED_EDGE('',*,*,#10717,.F.);
#14589=ORIENTED_EDGE('',*,*,#10794,.T.);
#14590=ORIENTED_EDGE('',*,*,#10795,.F.);
#14591=ORIENTED_EDGE('',*,*,#10793,.F.);
#14592=ORIENTED_EDGE('',*,*,#10796,.F.);
#14593=ORIENTED_EDGE('',*,*,#10790,.F.);
#14594=ORIENTED_EDGE('',*,*,#10716,.F.);
#14595=ORIENTED_EDGE('',*,*,#10797,.T.);
#14596=ORIENTED_EDGE('',*,*,#10798,.F.);
#14597=ORIENTED_EDGE('',*,*,#10794,.F.);
#14598=ORIENTED_EDGE('',*,*,#10799,.F.);
#14599=ORIENTED_EDGE('',*,*,#10800,.T.);
#14600=ORIENTED_EDGE('',*,*,#10715,.F.);
#14601=ORIENTED_EDGE('',*,*,#10801,.T.);
#14602=ORIENTED_EDGE('',*,*,#10802,.F.);
#14603=ORIENTED_EDGE('',*,*,#10800,.F.);
#14604=ORIENTED_EDGE('',*,*,#10803,.F.);
#14605=ORIENTED_EDGE('',*,*,#10797,.F.);
#14606=ORIENTED_EDGE('',*,*,#10714,.F.);
#14607=ORIENTED_EDGE('',*,*,#10804,.T.);
#14608=ORIENTED_EDGE('',*,*,#10805,.F.);
#14609=ORIENTED_EDGE('',*,*,#10801,.F.);
#14610=ORIENTED_EDGE('',*,*,#10806,.F.);
#14611=ORIENTED_EDGE('',*,*,#10807,.T.);
#14612=ORIENTED_EDGE('',*,*,#10713,.F.);
#14613=ORIENTED_EDGE('',*,*,#10808,.F.);
#14614=ORIENTED_EDGE('',*,*,#10809,.F.);
#14615=ORIENTED_EDGE('',*,*,#10807,.F.);
#14616=ORIENTED_EDGE('',*,*,#10810,.F.);
#14617=ORIENTED_EDGE('',*,*,#10804,.F.);
#14618=ORIENTED_EDGE('',*,*,#10811,.T.);
#14619=ORIENTED_EDGE('',*,*,#10812,.F.);
#14620=ORIENTED_EDGE('',*,*,#10808,.T.);
#14621=ORIENTED_EDGE('',*,*,#10712,.T.);
#14622=ORIENTED_EDGE('',*,*,#10813,.F.);
#14623=ORIENTED_EDGE('',*,*,#10814,.F.);
#14624=ORIENTED_EDGE('',*,*,#10811,.F.);
#14625=ORIENTED_EDGE('',*,*,#10711,.F.);
#14626=ORIENTED_EDGE('',*,*,#10667,.F.);
#14627=ORIENTED_EDGE('',*,*,#10670,.T.);
#14628=ORIENTED_EDGE('',*,*,#10673,.T.);
#14629=ORIENTED_EDGE('',*,*,#10674,.T.);
#14630=ORIENTED_EDGE('',*,*,#10815,.F.);
#14631=ORIENTED_EDGE('',*,*,#10816,.F.);
#14632=ORIENTED_EDGE('',*,*,#10813,.T.);
#14633=ORIENTED_EDGE('',*,*,#10817,.F.);
#14634=ORIENTED_EDGE('',*,*,#10393,.T.);
#14635=ORIENTED_EDGE('',*,*,#10818,.F.);
#14636=ORIENTED_EDGE('',*,*,#10815,.T.);
#14637=ORIENTED_EDGE('',*,*,#10676,.T.);
#14638=ORIENTED_EDGE('',*,*,#10710,.T.);
#14639=ORIENTED_EDGE('',*,*,#10819,.F.);
#14640=ORIENTED_EDGE('',*,*,#10820,.T.);
#14641=ORIENTED_EDGE('',*,*,#10736,.T.);
#14642=ORIENTED_EDGE('',*,*,#10821,.F.);
#14643=ORIENTED_EDGE('',*,*,#10822,.T.);
#14644=ORIENTED_EDGE('',*,*,#10701,.T.);
#14645=ORIENTED_EDGE('',*,*,#10817,.T.);
#14646=ORIENTED_EDGE('',*,*,#10709,.T.);
#14647=ORIENTED_EDGE('',*,*,#10823,.T.);
#14648=ORIENTED_EDGE('',*,*,#10824,.F.);
#14649=ORIENTED_EDGE('',*,*,#10825,.F.);
#14650=ORIENTED_EDGE('',*,*,#10826,.T.);
#14651=ORIENTED_EDGE('',*,*,#10827,.F.);
#14652=ORIENTED_EDGE('',*,*,#10823,.F.);
#14653=ORIENTED_EDGE('',*,*,#10708,.F.);
#14654=ORIENTED_EDGE('',*,*,#10828,.T.);
#14655=ORIENTED_EDGE('',*,*,#10829,.F.);
#14656=ORIENTED_EDGE('',*,*,#10826,.F.);
#14657=ORIENTED_EDGE('',*,*,#10707,.F.);
#14658=ORIENTED_EDGE('',*,*,#10830,.T.);
#14659=ORIENTED_EDGE('',*,*,#10831,.F.);
#14660=ORIENTED_EDGE('',*,*,#10828,.F.);
#14661=ORIENTED_EDGE('',*,*,#10832,.F.);
#14662=ORIENTED_EDGE('',*,*,#10833,.T.);
#14663=ORIENTED_EDGE('',*,*,#10706,.F.);
#14664=ORIENTED_EDGE('',*,*,#10834,.T.);
#14665=ORIENTED_EDGE('',*,*,#10835,.F.);
#14666=ORIENTED_EDGE('',*,*,#10833,.F.);
#14667=ORIENTED_EDGE('',*,*,#10836,.F.);
#14668=ORIENTED_EDGE('',*,*,#10830,.F.);
#14669=ORIENTED_EDGE('',*,*,#10705,.F.);
#14670=ORIENTED_EDGE('',*,*,#10837,.T.);
#14671=ORIENTED_EDGE('',*,*,#10838,.F.);
#14672=ORIENTED_EDGE('',*,*,#10834,.F.);
#14673=ORIENTED_EDGE('',*,*,#10839,.F.);
#14674=ORIENTED_EDGE('',*,*,#10840,.T.);
#14675=ORIENTED_EDGE('',*,*,#10704,.F.);
#14676=ORIENTED_EDGE('',*,*,#10841,.T.);
#14677=ORIENTED_EDGE('',*,*,#10842,.F.);
#14678=ORIENTED_EDGE('',*,*,#10840,.F.);
#14679=ORIENTED_EDGE('',*,*,#10843,.F.);
#14680=ORIENTED_EDGE('',*,*,#10837,.F.);
#14681=ORIENTED_EDGE('',*,*,#10703,.F.);
#14682=ORIENTED_EDGE('',*,*,#10844,.T.);
#14683=ORIENTED_EDGE('',*,*,#10845,.F.);
#14684=ORIENTED_EDGE('',*,*,#10841,.F.);
#14685=ORIENTED_EDGE('',*,*,#10702,.F.);
#14686=ORIENTED_EDGE('',*,*,#10822,.F.);
#14687=ORIENTED_EDGE('',*,*,#10846,.F.);
#14688=ORIENTED_EDGE('',*,*,#10820,.F.);
#14689=ORIENTED_EDGE('',*,*,#10847,.F.);
#14690=ORIENTED_EDGE('',*,*,#10844,.F.);
#14691=ORIENTED_EDGE('',*,*,#10732,.F.);
#14692=ORIENTED_EDGE('',*,*,#10730,.F.);
#14693=ORIENTED_EDGE('',*,*,#10728,.F.);
#14694=ORIENTED_EDGE('',*,*,#10726,.F.);
#14695=ORIENTED_EDGE('',*,*,#10724,.F.);
#14696=ORIENTED_EDGE('',*,*,#10722,.F.);
#14697=ORIENTED_EDGE('',*,*,#10719,.F.);
#14698=ORIENTED_EDGE('',*,*,#10734,.F.);
#14699=ORIENTED_EDGE('',*,*,#10848,.F.);
#14700=ORIENTED_EDGE('',*,*,#10849,.F.);
#14701=ORIENTED_EDGE('',*,*,#10850,.F.);
#14702=ORIENTED_EDGE('',*,*,#10851,.F.);
#14703=ORIENTED_EDGE('',*,*,#10852,.F.);
#14704=ORIENTED_EDGE('',*,*,#10853,.F.);
#14705=ORIENTED_EDGE('',*,*,#10854,.F.);
#14706=ORIENTED_EDGE('',*,*,#10855,.F.);
#14707=ORIENTED_EDGE('',*,*,#10856,.F.);
#14708=ORIENTED_EDGE('',*,*,#10857,.F.);
#14709=ORIENTED_EDGE('',*,*,#10423,.T.);
#14710=ORIENTED_EDGE('',*,*,#10858,.F.);
#14711=ORIENTED_EDGE('',*,*,#10859,.F.);
#14712=ORIENTED_EDGE('',*,*,#10858,.T.);
#14713=ORIENTED_EDGE('',*,*,#10738,.T.);
#14714=ORIENTED_EDGE('',*,*,#10860,.F.);
#14715=ORIENTED_EDGE('',*,*,#10861,.F.);
#14716=ORIENTED_EDGE('',*,*,#10860,.T.);
#14717=ORIENTED_EDGE('',*,*,#10421,.T.);
#14718=ORIENTED_EDGE('',*,*,#10862,.F.);
#14719=ORIENTED_EDGE('',*,*,#10863,.F.);
#14720=ORIENTED_EDGE('',*,*,#10864,.F.);
#14721=ORIENTED_EDGE('',*,*,#10862,.T.);
#14722=ORIENTED_EDGE('',*,*,#10741,.T.);
#14723=ORIENTED_EDGE('',*,*,#10744,.T.);
#14724=ORIENTED_EDGE('',*,*,#10742,.T.);
#14725=ORIENTED_EDGE('',*,*,#10746,.T.);
#14726=ORIENTED_EDGE('',*,*,#10748,.T.);
#14727=ORIENTED_EDGE('',*,*,#10753,.T.);
#14728=ORIENTED_EDGE('',*,*,#10749,.T.);
#14729=ORIENTED_EDGE('',*,*,#10752,.T.);
#14730=ORIENTED_EDGE('',*,*,#10755,.T.);
#14731=ORIENTED_EDGE('',*,*,#10760,.T.);
#14732=ORIENTED_EDGE('',*,*,#10756,.T.);
#14733=ORIENTED_EDGE('',*,*,#10759,.T.);
#14734=ORIENTED_EDGE('',*,*,#10762,.T.);
#14735=ORIENTED_EDGE('',*,*,#10767,.T.);
#14736=ORIENTED_EDGE('',*,*,#10763,.T.);
#14737=ORIENTED_EDGE('',*,*,#10766,.T.);
#14738=ORIENTED_EDGE('',*,*,#10768,.T.);
#14739=ORIENTED_EDGE('',*,*,#10865,.F.);
#14740=ORIENTED_EDGE('',*,*,#10863,.T.);
#14741=ORIENTED_EDGE('',*,*,#10415,.T.);
#14742=ORIENTED_EDGE('',*,*,#10866,.F.);
#14743=ORIENTED_EDGE('',*,*,#10867,.F.);
#14744=ORIENTED_EDGE('',*,*,#10866,.T.);
#14745=ORIENTED_EDGE('',*,*,#10769,.T.);
#14746=ORIENTED_EDGE('',*,*,#10868,.F.);
#14747=ORIENTED_EDGE('',*,*,#10869,.F.);
#14748=ORIENTED_EDGE('',*,*,#10868,.T.);
#14749=ORIENTED_EDGE('',*,*,#10409,.T.);
#14750=ORIENTED_EDGE('',*,*,#10367,.F.);
#14751=ORIENTED_EDGE('',*,*,#10870,.F.);
#14752=ORIENTED_EDGE('',*,*,#10365,.T.);
#14753=ORIENTED_EDGE('',*,*,#10396,.T.);
#14754=ORIENTED_EDGE('',*,*,#10871,.F.);
#14755=ORIENTED_EDGE('',*,*,#10872,.F.);
#14756=ORIENTED_EDGE('',*,*,#10871,.T.);
#14757=ORIENTED_EDGE('',*,*,#10781,.T.);
#14758=ORIENTED_EDGE('',*,*,#10873,.F.);
#14759=ORIENTED_EDGE('',*,*,#10874,.F.);
#14760=ORIENTED_EDGE('',*,*,#10873,.T.);
#14761=ORIENTED_EDGE('',*,*,#10782,.T.);
#14762=ORIENTED_EDGE('',*,*,#10875,.F.);
#14763=ORIENTED_EDGE('',*,*,#10876,.F.);
#14764=ORIENTED_EDGE('',*,*,#10877,.F.);
#14765=ORIENTED_EDGE('',*,*,#10875,.T.);
#14766=ORIENTED_EDGE('',*,*,#10784,.T.);
#14767=ORIENTED_EDGE('',*,*,#10787,.T.);
#14768=ORIENTED_EDGE('',*,*,#10785,.T.);
#14769=ORIENTED_EDGE('',*,*,#10789,.T.);
#14770=ORIENTED_EDGE('',*,*,#10791,.T.);
#14771=ORIENTED_EDGE('',*,*,#10796,.T.);
#14772=ORIENTED_EDGE('',*,*,#10792,.T.);
#14773=ORIENTED_EDGE('',*,*,#10795,.T.);
#14774=ORIENTED_EDGE('',*,*,#10798,.T.);
#14775=ORIENTED_EDGE('',*,*,#10803,.T.);
#14776=ORIENTED_EDGE('',*,*,#10799,.T.);
#14777=ORIENTED_EDGE('',*,*,#10802,.T.);
#14778=ORIENTED_EDGE('',*,*,#10805,.T.);
#14779=ORIENTED_EDGE('',*,*,#10810,.T.);
#14780=ORIENTED_EDGE('',*,*,#10806,.T.);
#14781=ORIENTED_EDGE('',*,*,#10809,.T.);
#14782=ORIENTED_EDGE('',*,*,#10812,.T.);
#14783=ORIENTED_EDGE('',*,*,#10878,.F.);
#14784=ORIENTED_EDGE('',*,*,#10876,.T.);
#14785=ORIENTED_EDGE('',*,*,#10814,.T.);
#14786=ORIENTED_EDGE('',*,*,#10879,.F.);
#14787=ORIENTED_EDGE('',*,*,#10880,.F.);
#14788=ORIENTED_EDGE('',*,*,#10879,.T.);
#14789=ORIENTED_EDGE('',*,*,#10816,.T.);
#14790=ORIENTED_EDGE('',*,*,#10881,.F.);
#14791=ORIENTED_EDGE('',*,*,#10882,.F.);
#14792=ORIENTED_EDGE('',*,*,#10881,.T.);
#14793=ORIENTED_EDGE('',*,*,#10818,.T.);
#14794=ORIENTED_EDGE('',*,*,#10394,.T.);
#14795=ORIENTED_EDGE('',*,*,#10883,.F.);
#14796=ORIENTED_EDGE('',*,*,#10845,.T.);
#14797=ORIENTED_EDGE('',*,*,#10847,.T.);
#14798=ORIENTED_EDGE('',*,*,#10819,.T.);
#14799=ORIENTED_EDGE('',*,*,#10846,.T.);
#14800=ORIENTED_EDGE('',*,*,#10821,.T.);
#14801=ORIENTED_EDGE('',*,*,#10857,.T.);
#14802=ORIENTED_EDGE('',*,*,#10884,.F.);
#14803=ORIENTED_EDGE('',*,*,#10883,.T.);
#14804=ORIENTED_EDGE('',*,*,#10824,.T.);
#14805=ORIENTED_EDGE('',*,*,#10827,.T.);
#14806=ORIENTED_EDGE('',*,*,#10825,.T.);
#14807=ORIENTED_EDGE('',*,*,#10829,.T.);
#14808=ORIENTED_EDGE('',*,*,#10831,.T.);
#14809=ORIENTED_EDGE('',*,*,#10836,.T.);
#14810=ORIENTED_EDGE('',*,*,#10832,.T.);
#14811=ORIENTED_EDGE('',*,*,#10835,.T.);
#14812=ORIENTED_EDGE('',*,*,#10838,.T.);
#14813=ORIENTED_EDGE('',*,*,#10843,.T.);
#14814=ORIENTED_EDGE('',*,*,#10839,.T.);
#14815=ORIENTED_EDGE('',*,*,#10842,.T.);
#14816=ORIENTED_EDGE('',*,*,#10885,.F.);
#14817=ORIENTED_EDGE('',*,*,#10852,.T.);
#14818=ORIENTED_EDGE('',*,*,#10886,.F.);
#14819=ORIENTED_EDGE('',*,*,#10887,.F.);
#14820=ORIENTED_EDGE('',*,*,#10888,.F.);
#14821=ORIENTED_EDGE('',*,*,#10854,.T.);
#14822=ORIENTED_EDGE('',*,*,#10889,.F.);
#14823=ORIENTED_EDGE('',*,*,#10890,.F.);
#14824=ORIENTED_EDGE('',*,*,#10378,.T.);
#14825=ORIENTED_EDGE('',*,*,#10381,.T.);
#14826=ORIENTED_EDGE('',*,*,#10891,.F.);
#14827=ORIENTED_EDGE('',*,*,#10892,.T.);
#14828=ORIENTED_EDGE('',*,*,#10893,.F.);
#14829=ORIENTED_EDGE('',*,*,#10889,.T.);
#14830=ORIENTED_EDGE('',*,*,#10853,.T.);
#14831=ORIENTED_EDGE('',*,*,#10885,.T.);
#14832=ORIENTED_EDGE('',*,*,#10894,.F.);
#14833=ORIENTED_EDGE('',*,*,#10848,.T.);
#14834=ORIENTED_EDGE('',*,*,#10895,.F.);
#14835=ORIENTED_EDGE('',*,*,#10896,.F.);
#14836=ORIENTED_EDGE('',*,*,#10855,.T.);
#14837=ORIENTED_EDGE('',*,*,#10888,.T.);
#14838=ORIENTED_EDGE('',*,*,#10897,.F.);
#14839=ORIENTED_EDGE('',*,*,#10898,.T.);
#14840=ORIENTED_EDGE('',*,*,#10899,.F.);
#14841=ORIENTED_EDGE('',*,*,#10895,.T.);
#14842=ORIENTED_EDGE('',*,*,#10900,.F.);
#14843=ORIENTED_EDGE('',*,*,#10901,.T.);
#14844=ORIENTED_EDGE('',*,*,#10902,.F.);
#14845=ORIENTED_EDGE('',*,*,#10903,.F.);
#14846=ORIENTED_EDGE('',*,*,#10849,.T.);
#14847=ORIENTED_EDGE('',*,*,#10894,.T.);
#14848=ORIENTED_EDGE('',*,*,#10851,.T.);
#14849=ORIENTED_EDGE('',*,*,#10904,.F.);
#14850=ORIENTED_EDGE('',*,*,#10905,.F.);
#14851=ORIENTED_EDGE('',*,*,#10906,.T.);
#14852=ORIENTED_EDGE('',*,*,#10907,.F.);
#14853=ORIENTED_EDGE('',*,*,#10886,.T.);
#14854=ORIENTED_EDGE('',*,*,#10904,.T.);
#14855=ORIENTED_EDGE('',*,*,#10850,.T.);
#14856=ORIENTED_EDGE('',*,*,#10903,.T.);
#14857=ORIENTED_EDGE('',*,*,#10908,.F.);
#14858=ORIENTED_EDGE('',*,*,#10909,.F.);
#14859=ORIENTED_EDGE('',*,*,#10910,.T.);
#14860=ORIENTED_EDGE('',*,*,#10911,.F.);
#14861=ORIENTED_EDGE('',*,*,#10912,.F.);
#14862=ORIENTED_EDGE('',*,*,#10913,.F.);
#14863=ORIENTED_EDGE('',*,*,#10914,.T.);
#14864=ORIENTED_EDGE('',*,*,#10915,.F.);
#14865=ORIENTED_EDGE('',*,*,#10910,.F.);
#14866=ORIENTED_EDGE('',*,*,#10914,.F.);
#14867=ORIENTED_EDGE('',*,*,#10916,.F.);
#14868=ORIENTED_EDGE('',*,*,#10917,.F.);
#14869=ORIENTED_EDGE('',*,*,#10918,.F.);
#14870=ORIENTED_EDGE('',*,*,#10919,.F.);
#14871=ORIENTED_EDGE('',*,*,#10920,.T.);
#14872=ORIENTED_EDGE('',*,*,#10921,.F.);
#14873=ORIENTED_EDGE('',*,*,#10922,.F.);
#14874=ORIENTED_EDGE('',*,*,#10923,.F.);
#14875=ORIENTED_EDGE('',*,*,#10924,.F.);
#14876=ORIENTED_EDGE('',*,*,#10919,.T.);
#14877=ORIENTED_EDGE('',*,*,#10925,.F.);
#14878=ORIENTED_EDGE('',*,*,#10926,.F.);
#14879=ORIENTED_EDGE('',*,*,#10927,.F.);
#14880=ORIENTED_EDGE('',*,*,#10928,.F.);
#14881=ORIENTED_EDGE('',*,*,#10923,.T.);
#14882=ORIENTED_EDGE('',*,*,#10929,.F.);
#14883=ORIENTED_EDGE('',*,*,#10930,.T.);
#14884=ORIENTED_EDGE('',*,*,#10931,.F.);
#14885=ORIENTED_EDGE('',*,*,#10932,.F.);
#14886=ORIENTED_EDGE('',*,*,#10933,.F.);
#14887=ORIENTED_EDGE('',*,*,#10934,.F.);
#14888=ORIENTED_EDGE('',*,*,#10929,.T.);
#14889=ORIENTED_EDGE('',*,*,#10935,.F.);
#14890=ORIENTED_EDGE('',*,*,#10936,.F.);
#14891=ORIENTED_EDGE('',*,*,#10937,.F.);
#14892=ORIENTED_EDGE('',*,*,#10938,.F.);
#14893=ORIENTED_EDGE('',*,*,#10933,.T.);
#14894=ORIENTED_EDGE('',*,*,#10939,.F.);
#14895=ORIENTED_EDGE('',*,*,#10940,.T.);
#14896=ORIENTED_EDGE('',*,*,#10941,.F.);
#14897=ORIENTED_EDGE('',*,*,#10942,.F.);
#14898=ORIENTED_EDGE('',*,*,#10943,.F.);
#14899=ORIENTED_EDGE('',*,*,#10944,.T.);
#14900=ORIENTED_EDGE('',*,*,#10945,.F.);
#14901=ORIENTED_EDGE('',*,*,#10940,.F.);
#14902=ORIENTED_EDGE('',*,*,#10944,.F.);
#14903=ORIENTED_EDGE('',*,*,#10946,.F.);
#14904=ORIENTED_EDGE('',*,*,#10947,.F.);
#14905=ORIENTED_EDGE('',*,*,#10948,.F.);
#14906=ORIENTED_EDGE('',*,*,#10346,.F.);
#14907=ORIENTED_EDGE('',*,*,#10949,.F.);
#14908=ORIENTED_EDGE('',*,*,#10926,.T.);
#14909=ORIENTED_EDGE('',*,*,#10925,.T.);
#14910=ORIENTED_EDGE('',*,*,#10922,.T.);
#14911=ORIENTED_EDGE('',*,*,#10950,.F.);
#14912=ORIENTED_EDGE('',*,*,#10951,.F.);
#14913=ORIENTED_EDGE('',*,*,#10952,.F.);
#14914=ORIENTED_EDGE('',*,*,#10916,.T.);
#14915=ORIENTED_EDGE('',*,*,#10913,.T.);
#14916=ORIENTED_EDGE('',*,*,#10909,.T.);
#14917=ORIENTED_EDGE('',*,*,#10953,.F.);
#14918=ORIENTED_EDGE('',*,*,#10954,.F.);
#14919=ORIENTED_EDGE('',*,*,#10955,.F.);
#14920=ORIENTED_EDGE('',*,*,#10946,.T.);
#14921=ORIENTED_EDGE('',*,*,#10943,.T.);
#14922=ORIENTED_EDGE('',*,*,#10939,.T.);
#14923=ORIENTED_EDGE('',*,*,#10956,.F.);
#14924=ORIENTED_EDGE('',*,*,#10957,.F.);
#14925=ORIENTED_EDGE('',*,*,#10958,.F.);
#14926=ORIENTED_EDGE('',*,*,#10936,.T.);
#14927=ORIENTED_EDGE('',*,*,#10935,.T.);
#14928=ORIENTED_EDGE('',*,*,#10932,.T.);
#14929=ORIENTED_EDGE('',*,*,#10959,.F.);
#14930=ORIENTED_EDGE('',*,*,#10882,.T.);
#14931=ORIENTED_EDGE('',*,*,#10884,.T.);
#14932=ORIENTED_EDGE('',*,*,#10856,.T.);
#14933=ORIENTED_EDGE('',*,*,#10859,.T.);
#14934=ORIENTED_EDGE('',*,*,#10861,.T.);
#14935=ORIENTED_EDGE('',*,*,#10864,.T.);
#14936=ORIENTED_EDGE('',*,*,#10865,.T.);
#14937=ORIENTED_EDGE('',*,*,#10867,.T.);
#14938=ORIENTED_EDGE('',*,*,#10869,.T.);
#14939=ORIENTED_EDGE('',*,*,#10366,.T.);
#14940=ORIENTED_EDGE('',*,*,#10870,.T.);
#14941=ORIENTED_EDGE('',*,*,#10872,.T.);
#14942=ORIENTED_EDGE('',*,*,#10874,.T.);
#14943=ORIENTED_EDGE('',*,*,#10877,.T.);
#14944=ORIENTED_EDGE('',*,*,#10878,.T.);
#14945=ORIENTED_EDGE('',*,*,#10880,.T.);
#14946=ORIENTED_EDGE('',*,*,#10960,.T.);
#14947=ORIENTED_EDGE('',*,*,#10961,.T.);
#14948=ORIENTED_EDGE('',*,*,#10962,.T.);
#14949=ORIENTED_EDGE('',*,*,#10963,.T.);
#14950=ORIENTED_EDGE('',*,*,#10964,.T.);
#14951=ORIENTED_EDGE('',*,*,#10965,.T.);
#14952=ORIENTED_EDGE('',*,*,#10966,.T.);
#14953=ORIENTED_EDGE('',*,*,#10967,.T.);
#14954=ORIENTED_EDGE('',*,*,#10968,.T.);
#14955=ORIENTED_EDGE('',*,*,#10969,.T.);
#14956=ORIENTED_EDGE('',*,*,#10970,.T.);
#14957=ORIENTED_EDGE('',*,*,#10971,.T.);
#14958=ORIENTED_EDGE('',*,*,#10891,.T.);
#14959=ORIENTED_EDGE('',*,*,#10887,.T.);
#14960=ORIENTED_EDGE('',*,*,#10907,.T.);
#14961=ORIENTED_EDGE('',*,*,#10972,.T.);
#14962=ORIENTED_EDGE('',*,*,#10893,.T.);
#14963=ORIENTED_EDGE('',*,*,#10973,.T.);
#14964=ORIENTED_EDGE('',*,*,#10897,.T.);
#14965=ORIENTED_EDGE('',*,*,#10890,.T.);
#14966=ORIENTED_EDGE('',*,*,#10899,.T.);
#14967=ORIENTED_EDGE('',*,*,#10974,.T.);
#14968=ORIENTED_EDGE('',*,*,#10900,.T.);
#14969=ORIENTED_EDGE('',*,*,#10896,.T.);
#14970=ORIENTED_EDGE('',*,*,#10905,.T.);
#14971=ORIENTED_EDGE('',*,*,#10908,.T.);
#14972=ORIENTED_EDGE('',*,*,#10902,.T.);
#14973=ORIENTED_EDGE('',*,*,#10975,.T.);
#14974=ORIENTED_EDGE('',*,*,#10976,.F.);
#14975=ORIENTED_EDGE('',*,*,#10977,.F.);
#14976=ORIENTED_EDGE('',*,*,#10953,.T.);
#14977=ORIENTED_EDGE('',*,*,#10978,.F.);
#14978=ORIENTED_EDGE('',*,*,#10979,.F.);
#14979=ORIENTED_EDGE('',*,*,#10980,.F.);
#14980=ORIENTED_EDGE('',*,*,#10978,.T.);
#14981=ORIENTED_EDGE('',*,*,#10912,.T.);
#14982=ORIENTED_EDGE('',*,*,#10981,.F.);
#14983=ORIENTED_EDGE('',*,*,#10982,.F.);
#14984=ORIENTED_EDGE('',*,*,#10979,.T.);
#14985=ORIENTED_EDGE('',*,*,#10911,.T.);
#14986=ORIENTED_EDGE('',*,*,#10915,.T.);
#14987=ORIENTED_EDGE('',*,*,#10918,.T.);
#14988=ORIENTED_EDGE('',*,*,#10983,.F.);
#14989=ORIENTED_EDGE('',*,*,#10984,.F.);
#14990=ORIENTED_EDGE('',*,*,#10981,.T.);
#14991=ORIENTED_EDGE('',*,*,#10917,.T.);
#14992=ORIENTED_EDGE('',*,*,#10985,.F.);
#14993=ORIENTED_EDGE('',*,*,#10983,.T.);
#14994=ORIENTED_EDGE('',*,*,#10952,.T.);
#14995=ORIENTED_EDGE('',*,*,#10986,.F.);
#14996=ORIENTED_EDGE('',*,*,#10987,.F.);
#14997=ORIENTED_EDGE('',*,*,#10988,.F.);
#14998=ORIENTED_EDGE('',*,*,#10986,.T.);
#14999=ORIENTED_EDGE('',*,*,#10951,.T.);
#15000=ORIENTED_EDGE('',*,*,#10989,.F.);
#15001=ORIENTED_EDGE('',*,*,#10987,.T.);
#15002=ORIENTED_EDGE('',*,*,#10950,.T.);
#15003=ORIENTED_EDGE('',*,*,#10990,.F.);
#15004=ORIENTED_EDGE('',*,*,#10991,.F.);
#15005=ORIENTED_EDGE('',*,*,#10992,.F.);
#15006=ORIENTED_EDGE('',*,*,#10990,.T.);
#15007=ORIENTED_EDGE('',*,*,#10921,.T.);
#15008=ORIENTED_EDGE('',*,*,#10991,.T.);
#15009=ORIENTED_EDGE('',*,*,#10920,.F.);
#15010=ORIENTED_EDGE('',*,*,#10924,.T.);
#15011=ORIENTED_EDGE('',*,*,#10928,.T.);
#15012=ORIENTED_EDGE('',*,*,#10993,.F.);
#15013=ORIENTED_EDGE('',*,*,#10994,.F.);
#15014=ORIENTED_EDGE('',*,*,#10995,.F.);
#15015=ORIENTED_EDGE('',*,*,#10996,.F.);
#15016=ORIENTED_EDGE('',*,*,#10993,.T.);
#15017=ORIENTED_EDGE('',*,*,#10927,.T.);
#15018=ORIENTED_EDGE('',*,*,#10997,.F.);
#15019=ORIENTED_EDGE('',*,*,#10995,.T.);
#15020=ORIENTED_EDGE('',*,*,#10949,.T.);
#15021=ORIENTED_EDGE('',*,*,#10349,.F.);
#15022=ORIENTED_EDGE('',*,*,#10998,.F.);
#15023=ORIENTED_EDGE('',*,*,#10347,.T.);
#15024=ORIENTED_EDGE('',*,*,#10959,.T.);
#15025=ORIENTED_EDGE('',*,*,#10999,.F.);
#15026=ORIENTED_EDGE('',*,*,#11000,.F.);
#15027=ORIENTED_EDGE('',*,*,#11001,.F.);
#15028=ORIENTED_EDGE('',*,*,#10999,.T.);
#15029=ORIENTED_EDGE('',*,*,#10931,.T.);
#15030=ORIENTED_EDGE('',*,*,#11000,.T.);
#15031=ORIENTED_EDGE('',*,*,#10930,.F.);
#15032=ORIENTED_EDGE('',*,*,#10934,.T.);
#15033=ORIENTED_EDGE('',*,*,#10938,.T.);
#15034=ORIENTED_EDGE('',*,*,#11002,.F.);
#15035=ORIENTED_EDGE('',*,*,#11003,.F.);
#15036=ORIENTED_EDGE('',*,*,#11004,.F.);
#15037=ORIENTED_EDGE('',*,*,#11005,.F.);
#15038=ORIENTED_EDGE('',*,*,#11002,.T.);
#15039=ORIENTED_EDGE('',*,*,#10937,.T.);
#15040=ORIENTED_EDGE('',*,*,#11006,.F.);
#15041=ORIENTED_EDGE('',*,*,#11004,.T.);
#15042=ORIENTED_EDGE('',*,*,#10958,.T.);
#15043=ORIENTED_EDGE('',*,*,#11007,.F.);
#15044=ORIENTED_EDGE('',*,*,#11008,.F.);
#15045=ORIENTED_EDGE('',*,*,#11009,.F.);
#15046=ORIENTED_EDGE('',*,*,#11007,.T.);
#15047=ORIENTED_EDGE('',*,*,#10957,.T.);
#15048=ORIENTED_EDGE('',*,*,#11010,.F.);
#15049=ORIENTED_EDGE('',*,*,#11008,.T.);
#15050=ORIENTED_EDGE('',*,*,#10956,.T.);
#15051=ORIENTED_EDGE('',*,*,#11011,.F.);
#15052=ORIENTED_EDGE('',*,*,#11012,.F.);
#15053=ORIENTED_EDGE('',*,*,#11013,.F.);
#15054=ORIENTED_EDGE('',*,*,#11011,.T.);
#15055=ORIENTED_EDGE('',*,*,#10942,.T.);
#15056=ORIENTED_EDGE('',*,*,#11014,.F.);
#15057=ORIENTED_EDGE('',*,*,#11015,.F.);
#15058=ORIENTED_EDGE('',*,*,#11012,.T.);
#15059=ORIENTED_EDGE('',*,*,#10941,.T.);
#15060=ORIENTED_EDGE('',*,*,#10945,.T.);
#15061=ORIENTED_EDGE('',*,*,#10948,.T.);
#15062=ORIENTED_EDGE('',*,*,#11016,.F.);
#15063=ORIENTED_EDGE('',*,*,#11017,.F.);
#15064=ORIENTED_EDGE('',*,*,#11014,.T.);
#15065=ORIENTED_EDGE('',*,*,#10947,.T.);
#15066=ORIENTED_EDGE('',*,*,#11018,.F.);
#15067=ORIENTED_EDGE('',*,*,#11016,.T.);
#15068=ORIENTED_EDGE('',*,*,#10955,.T.);
#15069=ORIENTED_EDGE('',*,*,#11019,.F.);
#15070=ORIENTED_EDGE('',*,*,#11020,.F.);
#15071=ORIENTED_EDGE('',*,*,#11019,.T.);
#15072=ORIENTED_EDGE('',*,*,#10954,.T.);
#15073=ORIENTED_EDGE('',*,*,#10977,.T.);
#15074=ORIENTED_EDGE('',*,*,#11021,.T.);
#15075=ORIENTED_EDGE('',*,*,#10965,.F.);
#15076=ORIENTED_EDGE('',*,*,#11022,.T.);
#15077=ORIENTED_EDGE('',*,*,#11023,.F.);
#15078=ORIENTED_EDGE('',*,*,#11022,.F.);
#15079=ORIENTED_EDGE('',*,*,#10964,.F.);
#15080=ORIENTED_EDGE('',*,*,#11024,.T.);
#15081=ORIENTED_EDGE('',*,*,#11025,.F.);
#15082=ORIENTED_EDGE('',*,*,#11024,.F.);
#15083=ORIENTED_EDGE('',*,*,#10963,.F.);
#15084=ORIENTED_EDGE('',*,*,#11026,.T.);
#15085=ORIENTED_EDGE('',*,*,#11027,.F.);
#15086=ORIENTED_EDGE('',*,*,#11026,.F.);
#15087=ORIENTED_EDGE('',*,*,#10962,.F.);
#15088=ORIENTED_EDGE('',*,*,#11028,.T.);
#15089=ORIENTED_EDGE('',*,*,#11029,.F.);
#15090=ORIENTED_EDGE('',*,*,#11028,.F.);
#15091=ORIENTED_EDGE('',*,*,#10961,.F.);
#15092=ORIENTED_EDGE('',*,*,#11030,.T.);
#15093=ORIENTED_EDGE('',*,*,#11031,.F.);
#15094=ORIENTED_EDGE('',*,*,#11030,.F.);
#15095=ORIENTED_EDGE('',*,*,#10960,.F.);
#15096=ORIENTED_EDGE('',*,*,#11021,.F.);
#15097=ORIENTED_EDGE('',*,*,#11032,.F.);
#15098=ORIENTED_EDGE('',*,*,#11033,.T.);
#15099=ORIENTED_EDGE('',*,*,#10971,.F.);
#15100=ORIENTED_EDGE('',*,*,#11034,.T.);
#15101=ORIENTED_EDGE('',*,*,#11035,.F.);
#15102=ORIENTED_EDGE('',*,*,#11034,.F.);
#15103=ORIENTED_EDGE('',*,*,#10970,.F.);
#15104=ORIENTED_EDGE('',*,*,#11036,.T.);
#15105=ORIENTED_EDGE('',*,*,#11037,.F.);
#15106=ORIENTED_EDGE('',*,*,#11036,.F.);
#15107=ORIENTED_EDGE('',*,*,#10969,.F.);
#15108=ORIENTED_EDGE('',*,*,#11038,.T.);
#15109=ORIENTED_EDGE('',*,*,#11039,.F.);
#15110=ORIENTED_EDGE('',*,*,#11038,.F.);
#15111=ORIENTED_EDGE('',*,*,#10968,.F.);
#15112=ORIENTED_EDGE('',*,*,#11040,.T.);
#15113=ORIENTED_EDGE('',*,*,#11041,.F.);
#15114=ORIENTED_EDGE('',*,*,#11040,.F.);
#15115=ORIENTED_EDGE('',*,*,#10967,.F.);
#15116=ORIENTED_EDGE('',*,*,#11042,.T.);
#15117=ORIENTED_EDGE('',*,*,#11043,.F.);
#15118=ORIENTED_EDGE('',*,*,#11042,.F.);
#15119=ORIENTED_EDGE('',*,*,#10966,.F.);
#15120=ORIENTED_EDGE('',*,*,#11033,.F.);
#15121=ORIENTED_EDGE('',*,*,#11044,.F.);
#15122=ORIENTED_EDGE('',*,*,#11045,.F.);
#15123=ORIENTED_EDGE('',*,*,#11046,.F.);
#15124=ORIENTED_EDGE('',*,*,#11047,.T.);
#15125=ORIENTED_EDGE('',*,*,#11048,.F.);
#15126=ORIENTED_EDGE('',*,*,#11049,.T.);
#15127=ORIENTED_EDGE('',*,*,#11050,.F.);
#15128=ORIENTED_EDGE('',*,*,#11051,.F.);
#15129=ORIENTED_EDGE('',*,*,#11052,.F.);
#15130=ORIENTED_EDGE('',*,*,#10901,.F.);
#15131=ORIENTED_EDGE('',*,*,#10974,.F.);
#15132=ORIENTED_EDGE('',*,*,#10898,.F.);
#15133=ORIENTED_EDGE('',*,*,#10973,.F.);
#15134=ORIENTED_EDGE('',*,*,#10892,.F.);
#15135=ORIENTED_EDGE('',*,*,#10972,.F.);
#15136=ORIENTED_EDGE('',*,*,#10906,.F.);
#15137=ORIENTED_EDGE('',*,*,#10975,.F.);
#15138=ORIENTED_EDGE('',*,*,#11053,.T.);
#15139=ORIENTED_EDGE('',*,*,#11054,.T.);
#15140=ORIENTED_EDGE('',*,*,#11055,.T.);
#15141=ORIENTED_EDGE('',*,*,#11056,.T.);
#15142=ORIENTED_EDGE('',*,*,#11057,.F.);
#15143=ORIENTED_EDGE('',*,*,#11058,.F.);
#15144=ORIENTED_EDGE('',*,*,#11059,.F.);
#15145=ORIENTED_EDGE('',*,*,#11060,.T.);
#15146=ORIENTED_EDGE('',*,*,#11054,.F.);
#15147=ORIENTED_EDGE('',*,*,#11061,.T.);
#15148=ORIENTED_EDGE('',*,*,#11062,.F.);
#15149=ORIENTED_EDGE('',*,*,#11058,.T.);
#15150=ORIENTED_EDGE('',*,*,#11063,.F.);
#15151=ORIENTED_EDGE('',*,*,#11064,.F.);
#15152=ORIENTED_EDGE('',*,*,#11065,.T.);
#15153=ORIENTED_EDGE('',*,*,#11066,.F.);
#15154=ORIENTED_EDGE('',*,*,#11067,.F.);
#15155=ORIENTED_EDGE('',*,*,#11068,.F.);
#15156=ORIENTED_EDGE('',*,*,#11069,.F.);
#15157=ORIENTED_EDGE('',*,*,#11070,.F.);
#15158=ORIENTED_EDGE('',*,*,#11071,.T.);
#15159=ORIENTED_EDGE('',*,*,#11072,.F.);
#15160=ORIENTED_EDGE('',*,*,#11073,.T.);
#15161=ORIENTED_EDGE('',*,*,#11074,.F.);
#15162=ORIENTED_EDGE('',*,*,#11075,.F.);
#15163=ORIENTED_EDGE('',*,*,#11076,.F.);
#15164=ORIENTED_EDGE('',*,*,#11018,.T.);
#15165=ORIENTED_EDGE('',*,*,#11020,.T.);
#15166=ORIENTED_EDGE('',*,*,#10976,.T.);
#15167=ORIENTED_EDGE('',*,*,#10980,.T.);
#15168=ORIENTED_EDGE('',*,*,#10982,.T.);
#15169=ORIENTED_EDGE('',*,*,#10984,.T.);
#15170=ORIENTED_EDGE('',*,*,#10985,.T.);
#15171=ORIENTED_EDGE('',*,*,#10988,.T.);
#15172=ORIENTED_EDGE('',*,*,#10989,.T.);
#15173=ORIENTED_EDGE('',*,*,#10992,.T.);
#15174=ORIENTED_EDGE('',*,*,#10994,.T.);
#15175=ORIENTED_EDGE('',*,*,#10996,.T.);
#15176=ORIENTED_EDGE('',*,*,#10997,.T.);
#15177=ORIENTED_EDGE('',*,*,#10348,.T.);
#15178=ORIENTED_EDGE('',*,*,#10998,.T.);
#15179=ORIENTED_EDGE('',*,*,#11001,.T.);
#15180=ORIENTED_EDGE('',*,*,#11003,.T.);
#15181=ORIENTED_EDGE('',*,*,#11005,.T.);
#15182=ORIENTED_EDGE('',*,*,#11006,.T.);
#15183=ORIENTED_EDGE('',*,*,#11009,.T.);
#15184=ORIENTED_EDGE('',*,*,#11010,.T.);
#15185=ORIENTED_EDGE('',*,*,#11013,.T.);
#15186=ORIENTED_EDGE('',*,*,#11015,.T.);
#15187=ORIENTED_EDGE('',*,*,#11017,.T.);
#15188=ORIENTED_EDGE('',*,*,#11077,.F.);
#15189=ORIENTED_EDGE('',*,*,#11069,.T.);
#15190=ORIENTED_EDGE('',*,*,#11078,.F.);
#15191=ORIENTED_EDGE('',*,*,#11067,.T.);
#15192=ORIENTED_EDGE('',*,*,#11079,.F.);
#15193=ORIENTED_EDGE('',*,*,#11064,.T.);
#15194=ORIENTED_EDGE('',*,*,#11080,.F.);
#15195=ORIENTED_EDGE('',*,*,#11051,.T.);
#15196=ORIENTED_EDGE('',*,*,#11081,.F.);
#15197=ORIENTED_EDGE('',*,*,#11045,.T.);
#15198=ORIENTED_EDGE('',*,*,#11082,.F.);
#15199=ORIENTED_EDGE('',*,*,#11083,.F.);
#15200=ORIENTED_EDGE('',*,*,#11084,.F.);
#15201=ORIENTED_EDGE('',*,*,#10341,.F.);
#15202=ORIENTED_EDGE('',*,*,#11085,.F.);
#15203=ORIENTED_EDGE('',*,*,#11075,.T.);
#15204=ORIENTED_EDGE('',*,*,#11086,.T.);
#15205=ORIENTED_EDGE('',*,*,#11087,.F.);
#15206=ORIENTED_EDGE('',*,*,#11083,.T.);
#15207=ORIENTED_EDGE('',*,*,#11088,.F.);
#15208=ORIENTED_EDGE('',*,*,#10326,.F.);
#15209=ORIENTED_EDGE('',*,*,#11031,.T.);
#15210=ORIENTED_EDGE('',*,*,#11032,.T.);
#15211=ORIENTED_EDGE('',*,*,#11023,.T.);
#15212=ORIENTED_EDGE('',*,*,#11025,.T.);
#15213=ORIENTED_EDGE('',*,*,#11027,.T.);
#15214=ORIENTED_EDGE('',*,*,#11029,.T.);
#15215=ORIENTED_EDGE('',*,*,#10323,.F.);
#15216=ORIENTED_EDGE('',*,*,#11043,.T.);
#15217=ORIENTED_EDGE('',*,*,#11044,.T.);
#15218=ORIENTED_EDGE('',*,*,#11035,.T.);
#15219=ORIENTED_EDGE('',*,*,#11037,.T.);
#15220=ORIENTED_EDGE('',*,*,#11039,.T.);
#15221=ORIENTED_EDGE('',*,*,#11041,.T.);
#15222=ORIENTED_EDGE('',*,*,#11048,.T.);
#15223=ORIENTED_EDGE('',*,*,#11089,.T.);
#15224=ORIENTED_EDGE('',*,*,#11090,.T.);
#15225=ORIENTED_EDGE('',*,*,#11091,.T.);
#15226=ORIENTED_EDGE('',*,*,#11088,.T.);
#15227=ORIENTED_EDGE('',*,*,#11082,.T.);
#15228=ORIENTED_EDGE('',*,*,#11050,.T.);
#15229=ORIENTED_EDGE('',*,*,#11092,.T.);
#15230=ORIENTED_EDGE('',*,*,#11093,.T.);
#15231=ORIENTED_EDGE('',*,*,#11094,.T.);
#15232=ORIENTED_EDGE('',*,*,#11046,.T.);
#15233=ORIENTED_EDGE('',*,*,#11081,.T.);
#15234=ORIENTED_EDGE('',*,*,#11089,.F.);
#15235=ORIENTED_EDGE('',*,*,#11047,.F.);
#15236=ORIENTED_EDGE('',*,*,#11094,.F.);
#15237=ORIENTED_EDGE('',*,*,#11095,.T.);
#15238=ORIENTED_EDGE('',*,*,#11096,.F.);
#15239=ORIENTED_EDGE('',*,*,#11097,.T.);
#15240=ORIENTED_EDGE('',*,*,#11098,.T.);
#15241=ORIENTED_EDGE('',*,*,#11099,.T.);
#15242=ORIENTED_EDGE('',*,*,#11100,.F.);
#15243=ORIENTED_EDGE('',*,*,#11101,.T.);
#15244=ORIENTED_EDGE('',*,*,#11102,.T.);
#15245=ORIENTED_EDGE('',*,*,#11103,.F.);
#15246=ORIENTED_EDGE('',*,*,#11104,.T.);
#15247=ORIENTED_EDGE('',*,*,#11105,.T.);
#15248=ORIENTED_EDGE('',*,*,#11080,.T.);
#15249=ORIENTED_EDGE('',*,*,#11063,.T.);
#15250=ORIENTED_EDGE('',*,*,#11057,.T.);
#15251=ORIENTED_EDGE('',*,*,#11106,.T.);
#15252=ORIENTED_EDGE('',*,*,#11107,.T.);
#15253=ORIENTED_EDGE('',*,*,#11108,.T.);
#15254=ORIENTED_EDGE('',*,*,#11109,.T.);
#15255=ORIENTED_EDGE('',*,*,#11052,.T.);
#15256=ORIENTED_EDGE('',*,*,#11110,.T.);
#15257=ORIENTED_EDGE('',*,*,#11105,.F.);
#15258=ORIENTED_EDGE('',*,*,#11111,.T.);
#15259=ORIENTED_EDGE('',*,*,#11092,.F.);
#15260=ORIENTED_EDGE('',*,*,#11049,.F.);
#15261=ORIENTED_EDGE('',*,*,#11109,.F.);
#15262=ORIENTED_EDGE('',*,*,#10335,.F.);
#15263=ORIENTED_EDGE('',*,*,#11112,.F.);
#15264=ORIENTED_EDGE('',*,*,#11113,.F.);
#15265=ORIENTED_EDGE('',*,*,#11114,.T.);
#15266=ORIENTED_EDGE('',*,*,#11107,.F.);
#15267=ORIENTED_EDGE('',*,*,#11115,.T.);
#15268=ORIENTED_EDGE('',*,*,#11116,.T.);
#15269=ORIENTED_EDGE('',*,*,#11115,.F.);
#15270=ORIENTED_EDGE('',*,*,#11106,.F.);
#15271=ORIENTED_EDGE('',*,*,#11061,.F.);
#15272=ORIENTED_EDGE('',*,*,#11053,.F.);
#15273=ORIENTED_EDGE('',*,*,#11117,.T.);
#15274=ORIENTED_EDGE('',*,*,#11118,.T.);
#15275=ORIENTED_EDGE('',*,*,#11119,.T.);
#15276=ORIENTED_EDGE('',*,*,#11055,.F.);
#15277=ORIENTED_EDGE('',*,*,#11060,.F.);
#15278=ORIENTED_EDGE('',*,*,#11120,.F.);
#15279=ORIENTED_EDGE('',*,*,#11121,.T.);
#15280=ORIENTED_EDGE('',*,*,#11122,.T.);
#15281=ORIENTED_EDGE('',*,*,#11123,.T.);
#15282=ORIENTED_EDGE('',*,*,#11124,.T.);
#15283=ORIENTED_EDGE('',*,*,#11117,.F.);
#15284=ORIENTED_EDGE('',*,*,#11056,.F.);
#15285=ORIENTED_EDGE('',*,*,#11119,.F.);
#15286=ORIENTED_EDGE('',*,*,#11125,.T.);
#15287=ORIENTED_EDGE('',*,*,#11126,.T.);
#15288=ORIENTED_EDGE('',*,*,#11120,.T.);
#15289=ORIENTED_EDGE('',*,*,#11059,.T.);
#15290=ORIENTED_EDGE('',*,*,#11062,.T.);
#15291=ORIENTED_EDGE('',*,*,#11079,.T.);
#15292=ORIENTED_EDGE('',*,*,#11066,.T.);
#15293=ORIENTED_EDGE('',*,*,#11127,.T.);
#15294=ORIENTED_EDGE('',*,*,#11126,.F.);
#15295=ORIENTED_EDGE('',*,*,#11128,.T.);
#15296=ORIENTED_EDGE('',*,*,#11129,.F.);
#15297=ORIENTED_EDGE('',*,*,#11130,.T.);
#15298=ORIENTED_EDGE('',*,*,#11121,.F.);
#15299=ORIENTED_EDGE('',*,*,#11131,.T.);
#15300=ORIENTED_EDGE('',*,*,#11132,.F.);
#15301=ORIENTED_EDGE('',*,*,#11133,.T.);
#15302=ORIENTED_EDGE('',*,*,#11134,.T.);
#15303=ORIENTED_EDGE('',*,*,#11072,.T.);
#15304=ORIENTED_EDGE('',*,*,#11135,.T.);
#15305=ORIENTED_EDGE('',*,*,#11136,.T.);
#15306=ORIENTED_EDGE('',*,*,#11137,.T.);
#15307=ORIENTED_EDGE('',*,*,#11068,.T.);
#15308=ORIENTED_EDGE('',*,*,#11078,.T.);
#15309=ORIENTED_EDGE('',*,*,#11138,.T.);
#15310=ORIENTED_EDGE('',*,*,#11134,.F.);
#15311=ORIENTED_EDGE('',*,*,#11139,.T.);
#15312=ORIENTED_EDGE('',*,*,#11127,.F.);
#15313=ORIENTED_EDGE('',*,*,#11065,.F.);
#15314=ORIENTED_EDGE('',*,*,#11137,.F.);
#15315=ORIENTED_EDGE('',*,*,#10332,.F.);
#15316=ORIENTED_EDGE('',*,*,#11074,.T.);
#15317=ORIENTED_EDGE('',*,*,#11140,.T.);
#15318=ORIENTED_EDGE('',*,*,#11141,.T.);
#15319=ORIENTED_EDGE('',*,*,#11142,.T.);
#15320=ORIENTED_EDGE('',*,*,#11070,.T.);
#15321=ORIENTED_EDGE('',*,*,#11077,.T.);
#15322=ORIENTED_EDGE('',*,*,#11135,.F.);
#15323=ORIENTED_EDGE('',*,*,#11071,.F.);
#15324=ORIENTED_EDGE('',*,*,#11142,.F.);
#15325=ORIENTED_EDGE('',*,*,#11143,.T.);
#15326=ORIENTED_EDGE('',*,*,#11144,.F.);
#15327=ORIENTED_EDGE('',*,*,#11145,.T.);
#15328=ORIENTED_EDGE('',*,*,#11146,.T.);
#15329=ORIENTED_EDGE('',*,*,#11147,.T.);
#15330=ORIENTED_EDGE('',*,*,#11148,.F.);
#15331=ORIENTED_EDGE('',*,*,#11149,.T.);
#15332=ORIENTED_EDGE('',*,*,#11150,.T.);
#15333=ORIENTED_EDGE('',*,*,#11151,.F.);
#15334=ORIENTED_EDGE('',*,*,#11152,.T.);
#15335=ORIENTED_EDGE('',*,*,#11153,.T.);
#15336=ORIENTED_EDGE('',*,*,#10340,.T.);
#15337=ORIENTED_EDGE('',*,*,#11154,.T.);
#15338=ORIENTED_EDGE('',*,*,#11155,.T.);
#15339=ORIENTED_EDGE('',*,*,#11156,.T.);
#15340=ORIENTED_EDGE('',*,*,#11076,.T.);
#15341=ORIENTED_EDGE('',*,*,#11085,.T.);
#15342=ORIENTED_EDGE('',*,*,#11157,.T.);
#15343=ORIENTED_EDGE('',*,*,#11153,.F.);
#15344=ORIENTED_EDGE('',*,*,#11158,.T.);
#15345=ORIENTED_EDGE('',*,*,#11140,.F.);
#15346=ORIENTED_EDGE('',*,*,#11073,.F.);
#15347=ORIENTED_EDGE('',*,*,#11156,.F.);
#15348=ORIENTED_EDGE('',*,*,#10329,.F.);
#15349=ORIENTED_EDGE('',*,*,#11159,.T.);
#15350=ORIENTED_EDGE('',*,*,#11160,.F.);
#15351=ORIENTED_EDGE('',*,*,#11161,.T.);
#15352=ORIENTED_EDGE('',*,*,#11162,.T.);
#15353=ORIENTED_EDGE('',*,*,#11163,.T.);
#15354=ORIENTED_EDGE('',*,*,#11162,.F.);
#15355=ORIENTED_EDGE('',*,*,#11164,.T.);
#15356=ORIENTED_EDGE('',*,*,#11165,.F.);
#15357=ORIENTED_EDGE('',*,*,#11086,.F.);
#15358=ORIENTED_EDGE('',*,*,#11091,.F.);
#15359=ORIENTED_EDGE('',*,*,#10338,.F.);
#15360=ORIENTED_EDGE('',*,*,#11087,.T.);
#15361=ORIENTED_EDGE('',*,*,#11165,.T.);
#15362=ORIENTED_EDGE('',*,*,#11166,.T.);
#15363=ORIENTED_EDGE('',*,*,#11167,.T.);
#15364=ORIENTED_EDGE('',*,*,#10342,.T.);
#15365=ORIENTED_EDGE('',*,*,#11084,.T.);
#15366=ORIENTED_EDGE('',*,*,#10339,.F.);
#15367=ORIENTED_EDGE('',*,*,#11167,.F.);
#15368=ORIENTED_EDGE('',*,*,#11168,.T.);
#15369=ORIENTED_EDGE('',*,*,#11169,.F.);
#15370=ORIENTED_EDGE('',*,*,#11170,.T.);
#15371=ORIENTED_EDGE('',*,*,#11171,.T.);
#15372=ORIENTED_EDGE('',*,*,#11172,.T.);
#15373=ORIENTED_EDGE('',*,*,#11173,.F.);
#15374=ORIENTED_EDGE('',*,*,#11174,.T.);
#15375=ORIENTED_EDGE('',*,*,#11154,.F.);
#15376=ORIENTED_EDGE('',*,*,#11175,.T.);
#15377=ORIENTED_EDGE('',*,*,#11176,.T.);
#15378=ORIENTED_EDGE('',*,*,#11177,.T.);
#15379=ORIENTED_EDGE('',*,*,#11178,.T.);
#15380=ORIENTED_EDGE('',*,*,#11179,.T.);
#15381=ORIENTED_EDGE('',*,*,#11180,.T.);
#15382=ORIENTED_EDGE('',*,*,#11181,.T.);
#15383=ORIENTED_EDGE('',*,*,#11182,.T.);
#15384=ORIENTED_EDGE('',*,*,#11183,.F.);
#15385=ORIENTED_EDGE('',*,*,#11184,.T.);
#15386=ORIENTED_EDGE('',*,*,#10320,.F.);
#15387=ORIENTED_EDGE('',*,*,#10131,.T.);
#15388=ORIENTED_EDGE('',*,*,#11185,.T.);
#15389=ORIENTED_EDGE('',*,*,#11186,.T.);
#15390=ORIENTED_EDGE('',*,*,#11160,.T.);
#15391=ORIENTED_EDGE('',*,*,#11187,.T.);
#15392=ORIENTED_EDGE('',*,*,#11188,.T.);
#15393=ORIENTED_EDGE('',*,*,#11189,.F.);
#15394=ORIENTED_EDGE('',*,*,#10336,.T.);
#15395=ORIENTED_EDGE('',*,*,#11189,.T.);
#15396=ORIENTED_EDGE('',*,*,#11190,.T.);
#15397=ORIENTED_EDGE('',*,*,#11191,.T.);
#15398=ORIENTED_EDGE('',*,*,#11192,.T.);
#15399=ORIENTED_EDGE('',*,*,#11090,.F.);
#15400=ORIENTED_EDGE('',*,*,#11101,.F.);
#15401=ORIENTED_EDGE('',*,*,#11193,.F.);
#15402=ORIENTED_EDGE('',*,*,#11194,.F.);
#15403=ORIENTED_EDGE('',*,*,#11195,.T.);
#15404=ORIENTED_EDGE('',*,*,#11187,.F.);
#15405=ORIENTED_EDGE('',*,*,#11159,.F.);
#15406=ORIENTED_EDGE('',*,*,#11163,.F.);
#15407=ORIENTED_EDGE('',*,*,#11100,.T.);
#15408=ORIENTED_EDGE('',*,*,#11196,.T.);
#15409=ORIENTED_EDGE('',*,*,#11197,.F.);
#15410=ORIENTED_EDGE('',*,*,#11193,.T.);
#15411=ORIENTED_EDGE('',*,*,#11196,.F.);
#15412=ORIENTED_EDGE('',*,*,#11099,.F.);
#15413=ORIENTED_EDGE('',*,*,#11198,.T.);
#15414=ORIENTED_EDGE('',*,*,#11199,.F.);
#15415=ORIENTED_EDGE('',*,*,#11198,.F.);
#15416=ORIENTED_EDGE('',*,*,#11098,.F.);
#15417=ORIENTED_EDGE('',*,*,#11200,.T.);
#15418=ORIENTED_EDGE('',*,*,#11201,.F.);
#15419=ORIENTED_EDGE('',*,*,#11200,.F.);
#15420=ORIENTED_EDGE('',*,*,#11097,.F.);
#15421=ORIENTED_EDGE('',*,*,#11202,.F.);
#15422=ORIENTED_EDGE('',*,*,#11203,.F.);
#15423=ORIENTED_EDGE('',*,*,#11096,.T.);
#15424=ORIENTED_EDGE('',*,*,#11204,.T.);
#15425=ORIENTED_EDGE('',*,*,#11205,.F.);
#15426=ORIENTED_EDGE('',*,*,#11202,.T.);
#15427=ORIENTED_EDGE('',*,*,#11093,.F.);
#15428=ORIENTED_EDGE('',*,*,#11111,.F.);
#15429=ORIENTED_EDGE('',*,*,#11104,.F.);
#15430=ORIENTED_EDGE('',*,*,#11206,.F.);
#15431=ORIENTED_EDGE('',*,*,#11207,.T.);
#15432=ORIENTED_EDGE('',*,*,#11208,.F.);
#15433=ORIENTED_EDGE('',*,*,#11204,.F.);
#15434=ORIENTED_EDGE('',*,*,#11095,.F.);
#15435=ORIENTED_EDGE('',*,*,#11209,.T.);
#15436=ORIENTED_EDGE('',*,*,#11206,.T.);
#15437=ORIENTED_EDGE('',*,*,#11103,.T.);
#15438=ORIENTED_EDGE('',*,*,#11210,.T.);
#15439=ORIENTED_EDGE('',*,*,#11211,.T.);
#15440=ORIENTED_EDGE('',*,*,#11212,.F.);
#15441=ORIENTED_EDGE('',*,*,#10333,.T.);
#15442=ORIENTED_EDGE('',*,*,#11212,.T.);
#15443=ORIENTED_EDGE('',*,*,#11213,.T.);
#15444=ORIENTED_EDGE('',*,*,#11214,.T.);
#15445=ORIENTED_EDGE('',*,*,#11215,.T.);
#15446=ORIENTED_EDGE('',*,*,#11108,.F.);
#15447=ORIENTED_EDGE('',*,*,#11114,.F.);
#15448=ORIENTED_EDGE('',*,*,#11216,.F.);
#15449=ORIENTED_EDGE('',*,*,#11217,.F.);
#15450=ORIENTED_EDGE('',*,*,#11218,.T.);
#15451=ORIENTED_EDGE('',*,*,#11210,.F.);
#15452=ORIENTED_EDGE('',*,*,#11102,.F.);
#15453=ORIENTED_EDGE('',*,*,#11110,.F.);
#15454=ORIENTED_EDGE('',*,*,#11113,.T.);
#15455=ORIENTED_EDGE('',*,*,#11219,.T.);
#15456=ORIENTED_EDGE('',*,*,#11220,.F.);
#15457=ORIENTED_EDGE('',*,*,#11216,.T.);
#15458=ORIENTED_EDGE('',*,*,#11221,.T.);
#15459=ORIENTED_EDGE('',*,*,#11222,.F.);
#15460=ORIENTED_EDGE('',*,*,#11219,.F.);
#15461=ORIENTED_EDGE('',*,*,#11112,.T.);
#15462=ORIENTED_EDGE('',*,*,#11116,.F.);
#15463=ORIENTED_EDGE('',*,*,#11124,.F.);
#15464=ORIENTED_EDGE('',*,*,#11223,.T.);
#15465=ORIENTED_EDGE('',*,*,#11224,.F.);
#15466=ORIENTED_EDGE('',*,*,#11221,.F.);
#15467=ORIENTED_EDGE('',*,*,#11123,.F.);
#15468=ORIENTED_EDGE('',*,*,#11118,.F.);
#15469=ORIENTED_EDGE('',*,*,#11130,.F.);
#15470=ORIENTED_EDGE('',*,*,#11225,.F.);
#15471=ORIENTED_EDGE('',*,*,#11226,.F.);
#15472=ORIENTED_EDGE('',*,*,#11223,.F.);
#15473=ORIENTED_EDGE('',*,*,#11122,.F.);
#15474=ORIENTED_EDGE('',*,*,#11129,.T.);
#15475=ORIENTED_EDGE('',*,*,#11227,.T.);
#15476=ORIENTED_EDGE('',*,*,#11228,.F.);
#15477=ORIENTED_EDGE('',*,*,#11225,.T.);
#15478=ORIENTED_EDGE('',*,*,#11125,.F.);
#15479=ORIENTED_EDGE('',*,*,#11139,.F.);
#15480=ORIENTED_EDGE('',*,*,#11133,.F.);
#15481=ORIENTED_EDGE('',*,*,#11229,.F.);
#15482=ORIENTED_EDGE('',*,*,#11230,.T.);
#15483=ORIENTED_EDGE('',*,*,#11231,.F.);
#15484=ORIENTED_EDGE('',*,*,#11227,.F.);
#15485=ORIENTED_EDGE('',*,*,#11128,.F.);
#15486=ORIENTED_EDGE('',*,*,#11232,.T.);
#15487=ORIENTED_EDGE('',*,*,#11229,.T.);
#15488=ORIENTED_EDGE('',*,*,#11132,.T.);
#15489=ORIENTED_EDGE('',*,*,#11233,.T.);
#15490=ORIENTED_EDGE('',*,*,#11234,.T.);
#15491=ORIENTED_EDGE('',*,*,#11235,.F.);
#15492=ORIENTED_EDGE('',*,*,#10330,.T.);
#15493=ORIENTED_EDGE('',*,*,#11235,.T.);
#15494=ORIENTED_EDGE('',*,*,#11236,.T.);
#15495=ORIENTED_EDGE('',*,*,#11237,.T.);
#15496=ORIENTED_EDGE('',*,*,#11238,.T.);
#15497=ORIENTED_EDGE('',*,*,#11136,.F.);
#15498=ORIENTED_EDGE('',*,*,#11149,.F.);
#15499=ORIENTED_EDGE('',*,*,#11239,.F.);
#15500=ORIENTED_EDGE('',*,*,#11240,.F.);
#15501=ORIENTED_EDGE('',*,*,#11241,.T.);
#15502=ORIENTED_EDGE('',*,*,#11233,.F.);
#15503=ORIENTED_EDGE('',*,*,#11131,.F.);
#15504=ORIENTED_EDGE('',*,*,#11138,.F.);
#15505=ORIENTED_EDGE('',*,*,#11148,.T.);
#15506=ORIENTED_EDGE('',*,*,#11242,.T.);
#15507=ORIENTED_EDGE('',*,*,#11243,.F.);
#15508=ORIENTED_EDGE('',*,*,#11239,.T.);
#15509=ORIENTED_EDGE('',*,*,#11242,.F.);
#15510=ORIENTED_EDGE('',*,*,#11147,.F.);
#15511=ORIENTED_EDGE('',*,*,#11244,.T.);
#15512=ORIENTED_EDGE('',*,*,#11245,.F.);
#15513=ORIENTED_EDGE('',*,*,#11244,.F.);
#15514=ORIENTED_EDGE('',*,*,#11146,.F.);
#15515=ORIENTED_EDGE('',*,*,#11246,.T.);
#15516=ORIENTED_EDGE('',*,*,#11247,.F.);
#15517=ORIENTED_EDGE('',*,*,#11246,.F.);
#15518=ORIENTED_EDGE('',*,*,#11145,.F.);
#15519=ORIENTED_EDGE('',*,*,#11248,.F.);
#15520=ORIENTED_EDGE('',*,*,#11249,.F.);
#15521=ORIENTED_EDGE('',*,*,#11144,.T.);
#15522=ORIENTED_EDGE('',*,*,#11250,.T.);
#15523=ORIENTED_EDGE('',*,*,#11251,.F.);
#15524=ORIENTED_EDGE('',*,*,#11248,.T.);
#15525=ORIENTED_EDGE('',*,*,#11141,.F.);
#15526=ORIENTED_EDGE('',*,*,#11158,.F.);
#15527=ORIENTED_EDGE('',*,*,#11152,.F.);
#15528=ORIENTED_EDGE('',*,*,#11252,.F.);
#15529=ORIENTED_EDGE('',*,*,#11253,.T.);
#15530=ORIENTED_EDGE('',*,*,#11254,.F.);
#15531=ORIENTED_EDGE('',*,*,#11250,.F.);
#15532=ORIENTED_EDGE('',*,*,#11143,.F.);
#15533=ORIENTED_EDGE('',*,*,#11255,.T.);
#15534=ORIENTED_EDGE('',*,*,#11252,.T.);
#15535=ORIENTED_EDGE('',*,*,#11151,.T.);
#15536=ORIENTED_EDGE('',*,*,#11256,.T.);
#15537=ORIENTED_EDGE('',*,*,#11257,.T.);
#15538=ORIENTED_EDGE('',*,*,#11258,.F.);
#15539=ORIENTED_EDGE('',*,*,#10327,.T.);
#15540=ORIENTED_EDGE('',*,*,#11258,.T.);
#15541=ORIENTED_EDGE('',*,*,#11259,.T.);
#15542=ORIENTED_EDGE('',*,*,#11260,.T.);
#15543=ORIENTED_EDGE('',*,*,#11261,.T.);
#15544=ORIENTED_EDGE('',*,*,#11155,.F.);
#15545=ORIENTED_EDGE('',*,*,#11174,.F.);
#15546=ORIENTED_EDGE('',*,*,#11262,.F.);
#15547=ORIENTED_EDGE('',*,*,#11263,.F.);
#15548=ORIENTED_EDGE('',*,*,#11264,.T.);
#15549=ORIENTED_EDGE('',*,*,#11256,.F.);
#15550=ORIENTED_EDGE('',*,*,#11150,.F.);
#15551=ORIENTED_EDGE('',*,*,#11157,.F.);
#15552=ORIENTED_EDGE('',*,*,#11173,.T.);
#15553=ORIENTED_EDGE('',*,*,#11265,.T.);
#15554=ORIENTED_EDGE('',*,*,#11266,.F.);
#15555=ORIENTED_EDGE('',*,*,#11262,.T.);
#15556=ORIENTED_EDGE('',*,*,#11265,.F.);
#15557=ORIENTED_EDGE('',*,*,#11172,.F.);
#15558=ORIENTED_EDGE('',*,*,#11267,.T.);
#15559=ORIENTED_EDGE('',*,*,#11268,.F.);
#15560=ORIENTED_EDGE('',*,*,#11267,.F.);
#15561=ORIENTED_EDGE('',*,*,#11171,.F.);
#15562=ORIENTED_EDGE('',*,*,#11269,.T.);
#15563=ORIENTED_EDGE('',*,*,#11270,.F.);
#15564=ORIENTED_EDGE('',*,*,#11269,.F.);
#15565=ORIENTED_EDGE('',*,*,#11170,.F.);
#15566=ORIENTED_EDGE('',*,*,#11271,.F.);
#15567=ORIENTED_EDGE('',*,*,#11272,.F.);
#15568=ORIENTED_EDGE('',*,*,#11169,.T.);
#15569=ORIENTED_EDGE('',*,*,#11273,.T.);
#15570=ORIENTED_EDGE('',*,*,#11274,.F.);
#15571=ORIENTED_EDGE('',*,*,#11271,.T.);
#15572=ORIENTED_EDGE('',*,*,#11166,.F.);
#15573=ORIENTED_EDGE('',*,*,#11164,.F.);
#15574=ORIENTED_EDGE('',*,*,#11161,.F.);
#15575=ORIENTED_EDGE('',*,*,#11186,.F.);
#15576=ORIENTED_EDGE('',*,*,#11275,.T.);
#15577=ORIENTED_EDGE('',*,*,#11276,.F.);
#15578=ORIENTED_EDGE('',*,*,#11273,.F.);
#15579=ORIENTED_EDGE('',*,*,#11168,.F.);
#15580=ORIENTED_EDGE('',*,*,#11277,.T.);
#15581=ORIENTED_EDGE('',*,*,#11278,.F.);
#15582=ORIENTED_EDGE('',*,*,#11279,.T.);
#15583=ORIENTED_EDGE('',*,*,#11180,.F.);
#15584=ORIENTED_EDGE('',*,*,#11280,.T.);
#15585=ORIENTED_EDGE('',*,*,#11281,.F.);
#15586=ORIENTED_EDGE('',*,*,#11277,.F.);
#15587=ORIENTED_EDGE('',*,*,#11179,.F.);
#15588=ORIENTED_EDGE('',*,*,#11282,.T.);
#15589=ORIENTED_EDGE('',*,*,#11283,.F.);
#15590=ORIENTED_EDGE('',*,*,#11280,.F.);
#15591=ORIENTED_EDGE('',*,*,#11178,.F.);
#15592=ORIENTED_EDGE('',*,*,#11284,.T.);
#15593=ORIENTED_EDGE('',*,*,#11285,.F.);
#15594=ORIENTED_EDGE('',*,*,#11282,.F.);
#15595=ORIENTED_EDGE('',*,*,#11177,.F.);
#15596=ORIENTED_EDGE('',*,*,#11286,.T.);
#15597=ORIENTED_EDGE('',*,*,#11287,.F.);
#15598=ORIENTED_EDGE('',*,*,#11284,.F.);
#15599=ORIENTED_EDGE('',*,*,#11176,.F.);
#15600=ORIENTED_EDGE('',*,*,#11279,.F.);
#15601=ORIENTED_EDGE('',*,*,#11288,.F.);
#15602=ORIENTED_EDGE('',*,*,#11286,.F.);
#15603=ORIENTED_EDGE('',*,*,#11175,.F.);
#15604=ORIENTED_EDGE('',*,*,#10316,.T.);
#15605=ORIENTED_EDGE('',*,*,#10324,.T.);
#15606=ORIENTED_EDGE('',*,*,#10313,.T.);
#15607=ORIENTED_EDGE('',*,*,#10321,.T.);
#15608=ORIENTED_EDGE('',*,*,#11289,.F.);
#15609=ORIENTED_EDGE('',*,*,#11182,.F.);
#15610=ORIENTED_EDGE('',*,*,#11290,.T.);
#15611=ORIENTED_EDGE('',*,*,#10311,.F.);
#15612=ORIENTED_EDGE('',*,*,#11290,.F.);
#15613=ORIENTED_EDGE('',*,*,#11181,.F.);
#15614=ORIENTED_EDGE('',*,*,#11291,.T.);
#15615=ORIENTED_EDGE('',*,*,#10305,.F.);
#15616=ORIENTED_EDGE('',*,*,#10312,.F.);
#15617=ORIENTED_EDGE('',*,*,#11291,.F.);
#15618=ORIENTED_EDGE('',*,*,#11184,.F.);
#15619=ORIENTED_EDGE('',*,*,#11292,.F.);
#15620=ORIENTED_EDGE('',*,*,#10306,.F.);
#15621=ORIENTED_EDGE('',*,*,#11289,.T.);
#15622=ORIENTED_EDGE('',*,*,#10310,.F.);
#15623=ORIENTED_EDGE('',*,*,#10307,.F.);
#15624=ORIENTED_EDGE('',*,*,#11292,.T.);
#15625=ORIENTED_EDGE('',*,*,#11183,.T.);
#15626=ORIENTED_EDGE('',*,*,#10302,.T.);
#15627=ORIENTED_EDGE('',*,*,#10299,.T.);
#15628=ORIENTED_EDGE('',*,*,#10296,.T.);
#15629=ORIENTED_EDGE('',*,*,#10293,.T.);
#15630=ORIENTED_EDGE('',*,*,#11185,.F.);
#15631=ORIENTED_EDGE('',*,*,#11192,.F.);
#15632=ORIENTED_EDGE('',*,*,#11293,.T.);
#15633=ORIENTED_EDGE('',*,*,#11294,.F.);
#15634=ORIENTED_EDGE('',*,*,#11295,.F.);
#15635=ORIENTED_EDGE('',*,*,#11275,.F.);
#15636=ORIENTED_EDGE('',*,*,#11296,.F.);
#15637=ORIENTED_EDGE('',*,*,#11297,.F.);
#15638=ORIENTED_EDGE('',*,*,#11298,.F.);
#15639=ORIENTED_EDGE('',*,*,#11299,.F.);
#15640=ORIENTED_EDGE('',*,*,#11293,.F.);
#15641=ORIENTED_EDGE('',*,*,#11191,.F.);
#15642=ORIENTED_EDGE('',*,*,#11300,.T.);
#15643=ORIENTED_EDGE('',*,*,#11301,.F.);
#15644=ORIENTED_EDGE('',*,*,#11302,.F.);
#15645=ORIENTED_EDGE('',*,*,#11303,.F.);
#15646=ORIENTED_EDGE('',*,*,#11300,.F.);
#15647=ORIENTED_EDGE('',*,*,#11190,.F.);
#15648=ORIENTED_EDGE('',*,*,#11188,.F.);
#15649=ORIENTED_EDGE('',*,*,#11195,.F.);
#15650=ORIENTED_EDGE('',*,*,#11304,.T.);
#15651=ORIENTED_EDGE('',*,*,#11305,.F.);
#15652=ORIENTED_EDGE('',*,*,#11302,.T.);
#15653=ORIENTED_EDGE('',*,*,#11194,.T.);
#15654=ORIENTED_EDGE('',*,*,#11197,.T.);
#15655=ORIENTED_EDGE('',*,*,#11199,.T.);
#15656=ORIENTED_EDGE('',*,*,#11201,.T.);
#15657=ORIENTED_EDGE('',*,*,#11203,.T.);
#15658=ORIENTED_EDGE('',*,*,#11205,.T.);
#15659=ORIENTED_EDGE('',*,*,#11208,.T.);
#15660=ORIENTED_EDGE('',*,*,#11209,.F.);
#15661=ORIENTED_EDGE('',*,*,#11215,.F.);
#15662=ORIENTED_EDGE('',*,*,#11306,.T.);
#15663=ORIENTED_EDGE('',*,*,#11307,.F.);
#15664=ORIENTED_EDGE('',*,*,#11304,.F.);
#15665=ORIENTED_EDGE('',*,*,#11207,.F.);
#15666=ORIENTED_EDGE('',*,*,#11308,.F.);
#15667=ORIENTED_EDGE('',*,*,#11309,.F.);
#15668=ORIENTED_EDGE('',*,*,#11310,.F.);
#15669=ORIENTED_EDGE('',*,*,#11311,.F.);
#15670=ORIENTED_EDGE('',*,*,#11306,.F.);
#15671=ORIENTED_EDGE('',*,*,#11214,.F.);
#15672=ORIENTED_EDGE('',*,*,#11312,.T.);
#15673=ORIENTED_EDGE('',*,*,#10287,.F.);
#15674=ORIENTED_EDGE('',*,*,#11313,.F.);
#15675=ORIENTED_EDGE('',*,*,#10288,.F.);
#15676=ORIENTED_EDGE('',*,*,#11312,.F.);
#15677=ORIENTED_EDGE('',*,*,#11213,.F.);
#15678=ORIENTED_EDGE('',*,*,#11211,.F.);
#15679=ORIENTED_EDGE('',*,*,#11218,.F.);
#15680=ORIENTED_EDGE('',*,*,#11228,.T.);
#15681=ORIENTED_EDGE('',*,*,#11231,.T.);
#15682=ORIENTED_EDGE('',*,*,#11314,.T.);
#15683=ORIENTED_EDGE('',*,*,#10282,.F.);
#15684=ORIENTED_EDGE('',*,*,#11313,.T.);
#15685=ORIENTED_EDGE('',*,*,#11217,.T.);
#15686=ORIENTED_EDGE('',*,*,#11220,.T.);
#15687=ORIENTED_EDGE('',*,*,#11222,.T.);
#15688=ORIENTED_EDGE('',*,*,#11224,.T.);
#15689=ORIENTED_EDGE('',*,*,#11226,.T.);
#15690=ORIENTED_EDGE('',*,*,#11232,.F.);
#15691=ORIENTED_EDGE('',*,*,#11238,.F.);
#15692=ORIENTED_EDGE('',*,*,#11315,.T.);
#15693=ORIENTED_EDGE('',*,*,#10283,.F.);
#15694=ORIENTED_EDGE('',*,*,#11314,.F.);
#15695=ORIENTED_EDGE('',*,*,#11230,.F.);
#15696=ORIENTED_EDGE('',*,*,#11315,.F.);
#15697=ORIENTED_EDGE('',*,*,#11237,.F.);
#15698=ORIENTED_EDGE('',*,*,#11316,.T.);
#15699=ORIENTED_EDGE('',*,*,#11317,.F.);
#15700=ORIENTED_EDGE('',*,*,#11318,.F.);
#15701=ORIENTED_EDGE('',*,*,#11319,.F.);
#15702=ORIENTED_EDGE('',*,*,#11320,.F.);
#15703=ORIENTED_EDGE('',*,*,#10284,.F.);
#15704=ORIENTED_EDGE('',*,*,#11321,.F.);
#15705=ORIENTED_EDGE('',*,*,#11322,.F.);
#15706=ORIENTED_EDGE('',*,*,#11316,.F.);
#15707=ORIENTED_EDGE('',*,*,#11236,.F.);
#15708=ORIENTED_EDGE('',*,*,#11234,.F.);
#15709=ORIENTED_EDGE('',*,*,#11241,.F.);
#15710=ORIENTED_EDGE('',*,*,#11251,.T.);
#15711=ORIENTED_EDGE('',*,*,#11254,.T.);
#15712=ORIENTED_EDGE('',*,*,#11323,.T.);
#15713=ORIENTED_EDGE('',*,*,#11324,.F.);
#15714=ORIENTED_EDGE('',*,*,#11321,.T.);
#15715=ORIENTED_EDGE('',*,*,#11240,.T.);
#15716=ORIENTED_EDGE('',*,*,#11243,.T.);
#15717=ORIENTED_EDGE('',*,*,#11245,.T.);
#15718=ORIENTED_EDGE('',*,*,#11247,.T.);
#15719=ORIENTED_EDGE('',*,*,#11249,.T.);
#15720=ORIENTED_EDGE('',*,*,#11255,.F.);
#15721=ORIENTED_EDGE('',*,*,#11261,.F.);
#15722=ORIENTED_EDGE('',*,*,#11325,.T.);
#15723=ORIENTED_EDGE('',*,*,#11326,.F.);
#15724=ORIENTED_EDGE('',*,*,#11323,.F.);
#15725=ORIENTED_EDGE('',*,*,#11253,.F.);
#15726=ORIENTED_EDGE('',*,*,#11325,.F.);
#15727=ORIENTED_EDGE('',*,*,#11260,.F.);
#15728=ORIENTED_EDGE('',*,*,#11327,.T.);
#15729=ORIENTED_EDGE('',*,*,#11328,.F.);
#15730=ORIENTED_EDGE('',*,*,#11329,.F.);
#15731=ORIENTED_EDGE('',*,*,#11330,.F.);
#15732=ORIENTED_EDGE('',*,*,#11331,.F.);
#15733=ORIENTED_EDGE('',*,*,#11332,.F.);
#15734=ORIENTED_EDGE('',*,*,#11333,.F.);
#15735=ORIENTED_EDGE('',*,*,#11334,.F.);
#15736=ORIENTED_EDGE('',*,*,#11327,.F.);
#15737=ORIENTED_EDGE('',*,*,#11259,.F.);
#15738=ORIENTED_EDGE('',*,*,#11257,.F.);
#15739=ORIENTED_EDGE('',*,*,#11264,.F.);
#15740=ORIENTED_EDGE('',*,*,#11274,.T.);
#15741=ORIENTED_EDGE('',*,*,#11276,.T.);
#15742=ORIENTED_EDGE('',*,*,#11295,.T.);
#15743=ORIENTED_EDGE('',*,*,#11335,.F.);
#15744=ORIENTED_EDGE('',*,*,#11333,.T.);
#15745=ORIENTED_EDGE('',*,*,#11263,.T.);
#15746=ORIENTED_EDGE('',*,*,#11266,.T.);
#15747=ORIENTED_EDGE('',*,*,#11268,.T.);
#15748=ORIENTED_EDGE('',*,*,#11270,.T.);
#15749=ORIENTED_EDGE('',*,*,#11272,.T.);
#15750=ORIENTED_EDGE('',*,*,#10290,.F.);
#15751=ORIENTED_EDGE('',*,*,#11287,.T.);
#15752=ORIENTED_EDGE('',*,*,#11288,.T.);
#15753=ORIENTED_EDGE('',*,*,#11278,.T.);
#15754=ORIENTED_EDGE('',*,*,#11281,.T.);
#15755=ORIENTED_EDGE('',*,*,#11283,.T.);
#15756=ORIENTED_EDGE('',*,*,#11285,.T.);
#15757=ORIENTED_EDGE('',*,*,#11336,.T.);
#15758=ORIENTED_EDGE('',*,*,#11337,.T.);
#15759=ORIENTED_EDGE('',*,*,#11338,.T.);
#15760=ORIENTED_EDGE('',*,*,#11339,.T.);
#15761=ORIENTED_EDGE('',*,*,#11340,.T.);
#15762=ORIENTED_EDGE('',*,*,#11341,.T.);
#15763=ORIENTED_EDGE('',*,*,#11298,.T.);
#15764=ORIENTED_EDGE('',*,*,#11342,.F.);
#15765=ORIENTED_EDGE('',*,*,#10254,.F.);
#15766=ORIENTED_EDGE('',*,*,#11343,.T.);
#15767=ORIENTED_EDGE('',*,*,#11344,.F.);
#15768=ORIENTED_EDGE('',*,*,#10255,.F.);
#15769=ORIENTED_EDGE('',*,*,#11342,.T.);
#15770=ORIENTED_EDGE('',*,*,#11297,.T.);
#15771=ORIENTED_EDGE('',*,*,#11296,.T.);
#15772=ORIENTED_EDGE('',*,*,#11345,.F.);
#15773=ORIENTED_EDGE('',*,*,#10256,.F.);
#15774=ORIENTED_EDGE('',*,*,#11344,.T.);
#15775=ORIENTED_EDGE('',*,*,#11345,.T.);
#15776=ORIENTED_EDGE('',*,*,#11301,.T.);
#15777=ORIENTED_EDGE('',*,*,#11303,.T.);
#15778=ORIENTED_EDGE('',*,*,#11305,.T.);
#15779=ORIENTED_EDGE('',*,*,#11307,.T.);
#15780=ORIENTED_EDGE('',*,*,#11311,.T.);
#15781=ORIENTED_EDGE('',*,*,#11346,.F.);
#15782=ORIENTED_EDGE('',*,*,#10262,.F.);
#15783=ORIENTED_EDGE('',*,*,#10257,.F.);
#15784=ORIENTED_EDGE('',*,*,#11310,.T.);
#15785=ORIENTED_EDGE('',*,*,#11347,.F.);
#15786=ORIENTED_EDGE('',*,*,#10263,.F.);
#15787=ORIENTED_EDGE('',*,*,#11346,.T.);
#15788=ORIENTED_EDGE('',*,*,#11348,.F.);
#15789=ORIENTED_EDGE('',*,*,#10264,.F.);
#15790=ORIENTED_EDGE('',*,*,#11347,.T.);
#15791=ORIENTED_EDGE('',*,*,#11309,.T.);
#15792=ORIENTED_EDGE('',*,*,#11308,.T.);
#15793=ORIENTED_EDGE('',*,*,#10286,.F.);
#15794=ORIENTED_EDGE('',*,*,#10265,.F.);
#15795=ORIENTED_EDGE('',*,*,#11348,.T.);
#15796=ORIENTED_EDGE('',*,*,#11320,.T.);
#15797=ORIENTED_EDGE('',*,*,#11349,.F.);
#15798=ORIENTED_EDGE('',*,*,#10267,.F.);
#15799=ORIENTED_EDGE('',*,*,#10285,.T.);
#15800=ORIENTED_EDGE('',*,*,#11350,.F.);
#15801=ORIENTED_EDGE('',*,*,#10268,.F.);
#15802=ORIENTED_EDGE('',*,*,#11349,.T.);
#15803=ORIENTED_EDGE('',*,*,#11319,.T.);
#15804=ORIENTED_EDGE('',*,*,#11318,.T.);
#15805=ORIENTED_EDGE('',*,*,#11351,.F.);
#15806=ORIENTED_EDGE('',*,*,#10269,.F.);
#15807=ORIENTED_EDGE('',*,*,#11350,.T.);
#15808=ORIENTED_EDGE('',*,*,#11351,.T.);
#15809=ORIENTED_EDGE('',*,*,#11317,.T.);
#15810=ORIENTED_EDGE('',*,*,#11322,.T.);
#15811=ORIENTED_EDGE('',*,*,#11324,.T.);
#15812=ORIENTED_EDGE('',*,*,#11326,.T.);
#15813=ORIENTED_EDGE('',*,*,#11332,.T.);
#15814=ORIENTED_EDGE('',*,*,#11352,.F.);
#15815=ORIENTED_EDGE('',*,*,#10249,.F.);
#15816=ORIENTED_EDGE('',*,*,#11331,.T.);
#15817=ORIENTED_EDGE('',*,*,#11353,.F.);
#15818=ORIENTED_EDGE('',*,*,#10250,.F.);
#15819=ORIENTED_EDGE('',*,*,#11352,.T.);
#15820=ORIENTED_EDGE('',*,*,#11354,.F.);
#15821=ORIENTED_EDGE('',*,*,#10251,.F.);
#15822=ORIENTED_EDGE('',*,*,#11353,.T.);
#15823=ORIENTED_EDGE('',*,*,#11330,.T.);
#15824=ORIENTED_EDGE('',*,*,#11329,.T.);
#15825=ORIENTED_EDGE('',*,*,#11355,.F.);
#15826=ORIENTED_EDGE('',*,*,#10252,.F.);
#15827=ORIENTED_EDGE('',*,*,#11354,.T.);
#15828=ORIENTED_EDGE('',*,*,#11334,.T.);
#15829=ORIENTED_EDGE('',*,*,#11335,.T.);
#15830=ORIENTED_EDGE('',*,*,#11294,.T.);
#15831=ORIENTED_EDGE('',*,*,#11299,.T.);
#15832=ORIENTED_EDGE('',*,*,#11343,.F.);
#15833=ORIENTED_EDGE('',*,*,#10253,.F.);
#15834=ORIENTED_EDGE('',*,*,#11355,.T.);
#15835=ORIENTED_EDGE('',*,*,#11328,.T.);
#15836=ORIENTED_EDGE('',*,*,#11356,.F.);
#15837=ORIENTED_EDGE('',*,*,#11357,.F.);
#15838=ORIENTED_EDGE('',*,*,#11358,.F.);
#15839=ORIENTED_EDGE('',*,*,#11359,.F.);
#15840=ORIENTED_EDGE('',*,*,#11360,.F.);
#15841=ORIENTED_EDGE('',*,*,#11361,.F.);
#15842=ORIENTED_EDGE('',*,*,#11362,.F.);
#15843=ORIENTED_EDGE('',*,*,#11363,.F.);
#15844=ORIENTED_EDGE('',*,*,#10318,.F.);
#15845=ORIENTED_EDGE('',*,*,#11360,.T.);
#15846=ORIENTED_EDGE('',*,*,#11364,.F.);
#15847=ORIENTED_EDGE('',*,*,#10278,.T.);
#15848=ORIENTED_EDGE('',*,*,#11365,.F.);
#15849=ORIENTED_EDGE('',*,*,#10280,.T.);
#15850=ORIENTED_EDGE('',*,*,#11366,.F.);
#15851=ORIENTED_EDGE('',*,*,#11367,.F.);
#15852=ORIENTED_EDGE('',*,*,#11368,.F.);
#15853=ORIENTED_EDGE('',*,*,#11369,.F.);
#15854=ORIENTED_EDGE('',*,*,#11370,.F.);
#15855=ORIENTED_EDGE('',*,*,#11371,.F.);
#15856=ORIENTED_EDGE('',*,*,#11372,.T.);
#15857=ORIENTED_EDGE('',*,*,#11373,.F.);
#15858=ORIENTED_EDGE('',*,*,#11374,.F.);
#15859=ORIENTED_EDGE('',*,*,#11367,.T.);
#15860=ORIENTED_EDGE('',*,*,#11375,.F.);
#15861=ORIENTED_EDGE('',*,*,#10315,.T.);
#15862=ORIENTED_EDGE('',*,*,#11376,.T.);
#15863=ORIENTED_EDGE('',*,*,#11377,.T.);
#15864=ORIENTED_EDGE('',*,*,#11378,.T.);
#15865=ORIENTED_EDGE('',*,*,#11379,.T.);
#15866=ORIENTED_EDGE('',*,*,#11380,.T.);
#15867=ORIENTED_EDGE('',*,*,#11381,.T.);
#15868=ORIENTED_EDGE('',*,*,#10201,.T.);
#15869=ORIENTED_EDGE('',*,*,#10242,.T.);
#15870=ORIENTED_EDGE('',*,*,#10248,.T.);
#15871=ORIENTED_EDGE('',*,*,#11382,.T.);
#15872=ORIENTED_EDGE('',*,*,#11383,.T.);
#15873=ORIENTED_EDGE('',*,*,#11384,.T.);
#15874=ORIENTED_EDGE('',*,*,#11385,.T.);
#15875=ORIENTED_EDGE('',*,*,#11340,.F.);
#15876=ORIENTED_EDGE('',*,*,#11385,.F.);
#15877=ORIENTED_EDGE('',*,*,#11386,.T.);
#15878=ORIENTED_EDGE('',*,*,#11387,.T.);
#15879=ORIENTED_EDGE('',*,*,#11341,.F.);
#15880=ORIENTED_EDGE('',*,*,#11387,.F.);
#15881=ORIENTED_EDGE('',*,*,#11388,.T.);
#15882=ORIENTED_EDGE('',*,*,#11389,.T.);
#15883=ORIENTED_EDGE('',*,*,#11336,.F.);
#15884=ORIENTED_EDGE('',*,*,#11389,.F.);
#15885=ORIENTED_EDGE('',*,*,#11390,.T.);
#15886=ORIENTED_EDGE('',*,*,#11391,.T.);
#15887=ORIENTED_EDGE('',*,*,#11337,.F.);
#15888=ORIENTED_EDGE('',*,*,#11391,.F.);
#15889=ORIENTED_EDGE('',*,*,#11392,.T.);
#15890=ORIENTED_EDGE('',*,*,#11393,.T.);
#15891=ORIENTED_EDGE('',*,*,#11338,.F.);
#15892=ORIENTED_EDGE('',*,*,#11393,.F.);
#15893=ORIENTED_EDGE('',*,*,#11394,.T.);
#15894=ORIENTED_EDGE('',*,*,#11383,.F.);
#15895=ORIENTED_EDGE('',*,*,#11339,.F.);
#15896=ORIENTED_EDGE('',*,*,#11382,.F.);
#15897=ORIENTED_EDGE('',*,*,#10247,.T.);
#15898=ORIENTED_EDGE('',*,*,#11395,.F.);
#15899=ORIENTED_EDGE('',*,*,#11396,.T.);
#15900=ORIENTED_EDGE('',*,*,#11397,.F.);
#15901=ORIENTED_EDGE('',*,*,#10202,.T.);
#15902=ORIENTED_EDGE('',*,*,#11371,.T.);
#15903=ORIENTED_EDGE('',*,*,#11398,.F.);
#15904=ORIENTED_EDGE('',*,*,#10235,.T.);
#15905=ORIENTED_EDGE('',*,*,#11399,.F.);
#15906=ORIENTED_EDGE('',*,*,#10234,.F.);
#15907=ORIENTED_EDGE('',*,*,#10303,.T.);
#15908=ORIENTED_EDGE('',*,*,#10231,.T.);
#15909=ORIENTED_EDGE('',*,*,#10300,.T.);
#15910=ORIENTED_EDGE('',*,*,#10228,.T.);
#15911=ORIENTED_EDGE('',*,*,#10297,.T.);
#15912=ORIENTED_EDGE('',*,*,#10225,.T.);
#15913=ORIENTED_EDGE('',*,*,#10294,.T.);
#15914=ORIENTED_EDGE('',*,*,#10222,.T.);
#15915=ORIENTED_EDGE('',*,*,#10291,.T.);
#15916=ORIENTED_EDGE('',*,*,#11400,.T.);
#15917=ORIENTED_EDGE('',*,*,#11401,.F.);
#15918=ORIENTED_EDGE('',*,*,#11402,.T.);
#15919=ORIENTED_EDGE('',*,*,#11401,.T.);
#15920=ORIENTED_EDGE('',*,*,#11403,.T.);
#15921=ORIENTED_EDGE('',*,*,#10277,.F.);
#15922=ORIENTED_EDGE('',*,*,#10273,.F.);
#15923=ORIENTED_EDGE('',*,*,#11404,.T.);
#15924=ORIENTED_EDGE('',*,*,#11405,.T.);
#15925=ORIENTED_EDGE('',*,*,#11406,.T.);
#15926=ORIENTED_EDGE('',*,*,#11407,.T.);
#15927=ORIENTED_EDGE('',*,*,#11408,.T.);
#15928=ORIENTED_EDGE('',*,*,#11409,.T.);
#15929=ORIENTED_EDGE('',*,*,#11410,.T.);
#15930=ORIENTED_EDGE('',*,*,#11411,.T.);
#15931=ORIENTED_EDGE('',*,*,#11412,.T.);
#15932=ORIENTED_EDGE('',*,*,#11413,.T.);
#15933=ORIENTED_EDGE('',*,*,#11414,.T.);
#15934=ORIENTED_EDGE('',*,*,#11415,.T.);
#15935=ORIENTED_EDGE('',*,*,#11416,.T.);
#15936=ORIENTED_EDGE('',*,*,#11417,.T.);
#15937=ORIENTED_EDGE('',*,*,#11418,.T.);
#15938=ORIENTED_EDGE('',*,*,#11419,.T.);
#15939=ORIENTED_EDGE('',*,*,#11420,.T.);
#15940=ORIENTED_EDGE('',*,*,#11421,.T.);
#15941=ORIENTED_EDGE('',*,*,#11422,.F.);
#15942=ORIENTED_EDGE('',*,*,#11370,.T.);
#15943=ORIENTED_EDGE('',*,*,#11423,.F.);
#15944=ORIENTED_EDGE('',*,*,#11423,.T.);
#15945=ORIENTED_EDGE('',*,*,#11369,.T.);
#15946=ORIENTED_EDGE('',*,*,#11424,.F.);
#15947=ORIENTED_EDGE('',*,*,#11425,.F.);
#15948=ORIENTED_EDGE('',*,*,#11426,.F.);
#15949=ORIENTED_EDGE('',*,*,#11424,.T.);
#15950=ORIENTED_EDGE('',*,*,#11375,.T.);
#15951=ORIENTED_EDGE('',*,*,#11427,.F.);
#15952=ORIENTED_EDGE('',*,*,#11359,.T.);
#15953=ORIENTED_EDGE('',*,*,#11428,.F.);
#15954=ORIENTED_EDGE('',*,*,#11428,.T.);
#15955=ORIENTED_EDGE('',*,*,#11358,.T.);
#15956=ORIENTED_EDGE('',*,*,#11429,.F.);
#15957=ORIENTED_EDGE('',*,*,#11430,.F.);
#15958=ORIENTED_EDGE('',*,*,#11431,.F.);
#15959=ORIENTED_EDGE('',*,*,#11429,.T.);
#15960=ORIENTED_EDGE('',*,*,#11357,.T.);
#15961=ORIENTED_EDGE('',*,*,#10209,.T.);
#15962=ORIENTED_EDGE('',*,*,#11432,.F.);
#15963=ORIENTED_EDGE('',*,*,#11356,.T.);
#15964=ORIENTED_EDGE('',*,*,#11433,.F.);
#15965=ORIENTED_EDGE('',*,*,#11434,.F.);
#15966=ORIENTED_EDGE('',*,*,#11363,.T.);
#15967=ORIENTED_EDGE('',*,*,#11435,.F.);
#15968=ORIENTED_EDGE('',*,*,#11435,.T.);
#15969=ORIENTED_EDGE('',*,*,#11362,.T.);
#15970=ORIENTED_EDGE('',*,*,#11436,.F.);
#15971=ORIENTED_EDGE('',*,*,#11437,.F.);
#15972=ORIENTED_EDGE('',*,*,#11438,.F.);
#15973=ORIENTED_EDGE('',*,*,#11436,.T.);
#15974=ORIENTED_EDGE('',*,*,#11361,.T.);
#15975=ORIENTED_EDGE('',*,*,#11439,.F.);
#15976=ORIENTED_EDGE('',*,*,#11374,.T.);
#15977=ORIENTED_EDGE('',*,*,#11440,.F.);
#15978=ORIENTED_EDGE('',*,*,#11440,.T.);
#15979=ORIENTED_EDGE('',*,*,#11373,.T.);
#15980=ORIENTED_EDGE('',*,*,#11441,.F.);
#15981=ORIENTED_EDGE('',*,*,#11442,.F.);
#15982=ORIENTED_EDGE('',*,*,#11443,.F.);
#15983=ORIENTED_EDGE('',*,*,#11441,.T.);
#15984=ORIENTED_EDGE('',*,*,#11372,.F.);
#15985=ORIENTED_EDGE('',*,*,#11444,.T.);
#15986=ORIENTED_EDGE('',*,*,#11445,.F.);
#15987=ORIENTED_EDGE('',*,*,#11446,.T.);
#15988=ORIENTED_EDGE('',*,*,#11380,.F.);
#15989=ORIENTED_EDGE('',*,*,#11447,.T.);
#15990=ORIENTED_EDGE('',*,*,#11448,.F.);
#15991=ORIENTED_EDGE('',*,*,#11444,.F.);
#15992=ORIENTED_EDGE('',*,*,#11379,.F.);
#15993=ORIENTED_EDGE('',*,*,#11449,.T.);
#15994=ORIENTED_EDGE('',*,*,#11450,.F.);
#15995=ORIENTED_EDGE('',*,*,#11447,.F.);
#15996=ORIENTED_EDGE('',*,*,#11378,.F.);
#15997=ORIENTED_EDGE('',*,*,#11451,.T.);
#15998=ORIENTED_EDGE('',*,*,#11452,.F.);
#15999=ORIENTED_EDGE('',*,*,#11449,.F.);
#16000=ORIENTED_EDGE('',*,*,#11377,.F.);
#16001=ORIENTED_EDGE('',*,*,#11453,.T.);
#16002=ORIENTED_EDGE('',*,*,#11454,.F.);
#16003=ORIENTED_EDGE('',*,*,#11451,.F.);
#16004=ORIENTED_EDGE('',*,*,#11376,.F.);
#16005=ORIENTED_EDGE('',*,*,#11446,.F.);
#16006=ORIENTED_EDGE('',*,*,#11455,.F.);
#16007=ORIENTED_EDGE('',*,*,#11453,.F.);
#16008=ORIENTED_EDGE('',*,*,#11381,.F.);
#16009=ORIENTED_EDGE('',*,*,#11456,.F.);
#16010=ORIENTED_EDGE('',*,*,#10203,.T.);
#16011=ORIENTED_EDGE('',*,*,#11397,.T.);
#16012=ORIENTED_EDGE('',*,*,#11457,.T.);
#16013=ORIENTED_EDGE('',*,*,#11458,.F.);
#16014=ORIENTED_EDGE('',*,*,#11459,.T.);
#16015=ORIENTED_EDGE('',*,*,#11460,.F.);
#16016=ORIENTED_EDGE('',*,*,#11458,.T.);
#16017=ORIENTED_EDGE('',*,*,#11459,.F.);
#16018=ORIENTED_EDGE('',*,*,#11457,.F.);
#16019=ORIENTED_EDGE('',*,*,#11396,.F.);
#16020=ORIENTED_EDGE('',*,*,#11461,.F.);
#16021=ORIENTED_EDGE('',*,*,#11462,.F.);
#16022=ORIENTED_EDGE('',*,*,#11463,.F.);
#16023=ORIENTED_EDGE('',*,*,#11392,.F.);
#16024=ORIENTED_EDGE('',*,*,#11390,.F.);
#16025=ORIENTED_EDGE('',*,*,#11388,.F.);
#16026=ORIENTED_EDGE('',*,*,#11386,.F.);
#16027=ORIENTED_EDGE('',*,*,#11384,.F.);
#16028=ORIENTED_EDGE('',*,*,#11394,.F.);
#16029=ORIENTED_EDGE('',*,*,#11464,.F.);
#16030=ORIENTED_EDGE('',*,*,#11465,.F.);
#16031=ORIENTED_EDGE('',*,*,#11462,.T.);
#16032=ORIENTED_EDGE('',*,*,#11466,.F.);
#16033=ORIENTED_EDGE('',*,*,#11467,.F.);
#16034=ORIENTED_EDGE('',*,*,#11464,.T.);
#16035=ORIENTED_EDGE('',*,*,#11461,.T.);
#16036=ORIENTED_EDGE('',*,*,#11395,.T.);
#16037=ORIENTED_EDGE('',*,*,#10246,.T.);
#16038=ORIENTED_EDGE('',*,*,#11468,.T.);
#16039=ORIENTED_EDGE('',*,*,#11469,.T.);
#16040=ORIENTED_EDGE('',*,*,#11470,.T.);
#16041=ORIENTED_EDGE('',*,*,#11471,.T.);
#16042=ORIENTED_EDGE('',*,*,#11472,.T.);
#16043=ORIENTED_EDGE('',*,*,#11473,.T.);
#16044=ORIENTED_EDGE('',*,*,#11474,.T.);
#16045=ORIENTED_EDGE('',*,*,#11475,.T.);
#16046=ORIENTED_EDGE('',*,*,#11476,.T.);
#16047=ORIENTED_EDGE('',*,*,#11477,.T.);
#16048=ORIENTED_EDGE('',*,*,#11478,.T.);
#16049=ORIENTED_EDGE('',*,*,#11479,.T.);
#16050=ORIENTED_EDGE('',*,*,#11480,.T.);
#16051=ORIENTED_EDGE('',*,*,#11481,.T.);
#16052=ORIENTED_EDGE('',*,*,#11482,.T.);
#16053=ORIENTED_EDGE('',*,*,#11483,.T.);
#16054=ORIENTED_EDGE('',*,*,#11484,.T.);
#16055=ORIENTED_EDGE('',*,*,#11485,.T.);
#16056=ORIENTED_EDGE('',*,*,#11486,.T.);
#16057=ORIENTED_EDGE('',*,*,#11487,.T.);
#16058=ORIENTED_EDGE('',*,*,#10259,.T.);
#16059=ORIENTED_EDGE('',*,*,#10219,.T.);
#16060=ORIENTED_EDGE('',*,*,#10260,.F.);
#16061=ORIENTED_EDGE('',*,*,#11487,.F.);
#16062=ORIENTED_EDGE('',*,*,#11488,.T.);
#16063=ORIENTED_EDGE('',*,*,#11489,.T.);
#16064=ORIENTED_EDGE('',*,*,#10272,.F.);
#16065=ORIENTED_EDGE('',*,*,#11403,.F.);
#16066=ORIENTED_EDGE('',*,*,#11400,.F.);
#16067=ORIENTED_EDGE('',*,*,#11402,.F.);
#16068=ORIENTED_EDGE('',*,*,#10261,.F.);
#16069=ORIENTED_EDGE('',*,*,#11489,.F.);
#16070=ORIENTED_EDGE('',*,*,#11490,.T.);
#16071=ORIENTED_EDGE('',*,*,#10217,.F.);
#16072=ORIENTED_EDGE('',*,*,#11491,.T.);
#16073=ORIENTED_EDGE('',*,*,#11492,.T.);
#16074=ORIENTED_EDGE('',*,*,#11493,.T.);
#16075=ORIENTED_EDGE('',*,*,#11494,.T.);
#16076=ORIENTED_EDGE('',*,*,#11495,.T.);
#16077=ORIENTED_EDGE('',*,*,#11496,.T.);
#16078=ORIENTED_EDGE('',*,*,#11497,.T.);
#16079=ORIENTED_EDGE('',*,*,#11498,.T.);
#16080=ORIENTED_EDGE('',*,*,#11499,.T.);
#16081=ORIENTED_EDGE('',*,*,#11500,.T.);
#16082=ORIENTED_EDGE('',*,*,#11501,.T.);
#16083=ORIENTED_EDGE('',*,*,#11502,.T.);
#16084=ORIENTED_EDGE('',*,*,#11503,.T.);
#16085=ORIENTED_EDGE('',*,*,#11409,.F.);
#16086=ORIENTED_EDGE('',*,*,#11504,.T.);
#16087=ORIENTED_EDGE('',*,*,#11505,.F.);
#16088=ORIENTED_EDGE('',*,*,#11504,.F.);
#16089=ORIENTED_EDGE('',*,*,#11408,.F.);
#16090=ORIENTED_EDGE('',*,*,#11506,.T.);
#16091=ORIENTED_EDGE('',*,*,#11507,.F.);
#16092=ORIENTED_EDGE('',*,*,#11506,.F.);
#16093=ORIENTED_EDGE('',*,*,#11407,.F.);
#16094=ORIENTED_EDGE('',*,*,#11508,.T.);
#16095=ORIENTED_EDGE('',*,*,#11509,.F.);
#16096=ORIENTED_EDGE('',*,*,#11508,.F.);
#16097=ORIENTED_EDGE('',*,*,#11406,.F.);
#16098=ORIENTED_EDGE('',*,*,#11510,.T.);
#16099=ORIENTED_EDGE('',*,*,#11511,.F.);
#16100=ORIENTED_EDGE('',*,*,#11510,.F.);
#16101=ORIENTED_EDGE('',*,*,#11405,.F.);
#16102=ORIENTED_EDGE('',*,*,#11512,.T.);
#16103=ORIENTED_EDGE('',*,*,#11513,.F.);
#16104=ORIENTED_EDGE('',*,*,#11512,.F.);
#16105=ORIENTED_EDGE('',*,*,#11404,.F.);
#16106=ORIENTED_EDGE('',*,*,#11503,.F.);
#16107=ORIENTED_EDGE('',*,*,#11514,.F.);
#16108=ORIENTED_EDGE('',*,*,#11515,.T.);
#16109=ORIENTED_EDGE('',*,*,#11516,.F.);
#16110=ORIENTED_EDGE('',*,*,#11517,.T.);
#16111=ORIENTED_EDGE('',*,*,#11518,.F.);
#16112=ORIENTED_EDGE('',*,*,#11519,.T.);
#16113=ORIENTED_EDGE('',*,*,#11515,.F.);
#16114=ORIENTED_EDGE('',*,*,#11520,.T.);
#16115=ORIENTED_EDGE('',*,*,#11521,.T.);
#16116=ORIENTED_EDGE('',*,*,#11522,.T.);
#16117=ORIENTED_EDGE('',*,*,#11523,.F.);
#16118=ORIENTED_EDGE('',*,*,#11524,.T.);
#16119=ORIENTED_EDGE('',*,*,#11518,.T.);
#16120=ORIENTED_EDGE('',*,*,#11525,.T.);
#16121=ORIENTED_EDGE('',*,*,#11526,.T.);
#16122=ORIENTED_EDGE('',*,*,#11527,.T.);
#16123=ORIENTED_EDGE('',*,*,#11414,.F.);
#16124=ORIENTED_EDGE('',*,*,#11527,.F.);
#16125=ORIENTED_EDGE('',*,*,#11528,.T.);
#16126=ORIENTED_EDGE('',*,*,#11529,.T.);
#16127=ORIENTED_EDGE('',*,*,#11415,.F.);
#16128=ORIENTED_EDGE('',*,*,#11529,.F.);
#16129=ORIENTED_EDGE('',*,*,#11530,.T.);
#16130=ORIENTED_EDGE('',*,*,#11531,.T.);
#16131=ORIENTED_EDGE('',*,*,#11410,.F.);
#16132=ORIENTED_EDGE('',*,*,#11531,.F.);
#16133=ORIENTED_EDGE('',*,*,#11532,.T.);
#16134=ORIENTED_EDGE('',*,*,#11533,.T.);
#16135=ORIENTED_EDGE('',*,*,#11411,.F.);
#16136=ORIENTED_EDGE('',*,*,#11533,.F.);
#16137=ORIENTED_EDGE('',*,*,#11534,.T.);
#16138=ORIENTED_EDGE('',*,*,#11535,.T.);
#16139=ORIENTED_EDGE('',*,*,#11412,.F.);
#16140=ORIENTED_EDGE('',*,*,#11535,.F.);
#16141=ORIENTED_EDGE('',*,*,#11536,.T.);
#16142=ORIENTED_EDGE('',*,*,#11525,.F.);
#16143=ORIENTED_EDGE('',*,*,#11413,.F.);
#16144=ORIENTED_EDGE('',*,*,#11537,.F.);
#16145=ORIENTED_EDGE('',*,*,#11538,.T.);
#16146=ORIENTED_EDGE('',*,*,#11539,.F.);
#16147=ORIENTED_EDGE('',*,*,#11540,.F.);
#16148=ORIENTED_EDGE('',*,*,#11539,.T.);
#16149=ORIENTED_EDGE('',*,*,#11541,.T.);
#16150=ORIENTED_EDGE('',*,*,#11542,.F.);
#16151=ORIENTED_EDGE('',*,*,#11543,.T.);
#16152=ORIENTED_EDGE('',*,*,#11544,.F.);
#16153=ORIENTED_EDGE('',*,*,#11545,.T.);
#16154=ORIENTED_EDGE('',*,*,#11546,.F.);
#16155=ORIENTED_EDGE('',*,*,#11547,.T.);
#16156=ORIENTED_EDGE('',*,*,#11420,.F.);
#16157=ORIENTED_EDGE('',*,*,#11548,.T.);
#16158=ORIENTED_EDGE('',*,*,#11549,.F.);
#16159=ORIENTED_EDGE('',*,*,#11545,.F.);
#16160=ORIENTED_EDGE('',*,*,#11419,.F.);
#16161=ORIENTED_EDGE('',*,*,#11550,.T.);
#16162=ORIENTED_EDGE('',*,*,#11551,.F.);
#16163=ORIENTED_EDGE('',*,*,#11548,.F.);
#16164=ORIENTED_EDGE('',*,*,#11418,.F.);
#16165=ORIENTED_EDGE('',*,*,#11552,.T.);
#16166=ORIENTED_EDGE('',*,*,#11553,.F.);
#16167=ORIENTED_EDGE('',*,*,#11550,.F.);
#16168=ORIENTED_EDGE('',*,*,#11417,.F.);
#16169=ORIENTED_EDGE('',*,*,#11554,.T.);
#16170=ORIENTED_EDGE('',*,*,#11555,.F.);
#16171=ORIENTED_EDGE('',*,*,#11552,.F.);
#16172=ORIENTED_EDGE('',*,*,#11416,.F.);
#16173=ORIENTED_EDGE('',*,*,#11547,.F.);
#16174=ORIENTED_EDGE('',*,*,#11556,.F.);
#16175=ORIENTED_EDGE('',*,*,#11554,.F.);
#16176=ORIENTED_EDGE('',*,*,#11421,.F.);
#16177=ORIENTED_EDGE('',*,*,#11557,.T.);
#16178=ORIENTED_EDGE('',*,*,#11558,.F.);
#16179=ORIENTED_EDGE('',*,*,#10212,.T.);
#16180=ORIENTED_EDGE('',*,*,#11559,.F.);
#16181=ORIENTED_EDGE('',*,*,#10208,.T.);
#16182=ORIENTED_EDGE('',*,*,#11560,.F.);
#16183=ORIENTED_EDGE('',*,*,#11561,.F.);
#16184=ORIENTED_EDGE('',*,*,#10214,.T.);
#16185=ORIENTED_EDGE('',*,*,#11562,.F.);
#16186=ORIENTED_EDGE('',*,*,#11563,.F.);
#16187=ORIENTED_EDGE('',*,*,#10236,.T.);
#16188=ORIENTED_EDGE('',*,*,#11398,.T.);
#16189=ORIENTED_EDGE('',*,*,#11422,.T.);
#16190=ORIENTED_EDGE('',*,*,#11425,.T.);
#16191=ORIENTED_EDGE('',*,*,#11426,.T.);
#16192=ORIENTED_EDGE('',*,*,#11366,.T.);
#16193=ORIENTED_EDGE('',*,*,#10279,.T.);
#16194=ORIENTED_EDGE('',*,*,#11364,.T.);
#16195=ORIENTED_EDGE('',*,*,#11427,.T.);
#16196=ORIENTED_EDGE('',*,*,#11430,.T.);
#16197=ORIENTED_EDGE('',*,*,#11431,.T.);
#16198=ORIENTED_EDGE('',*,*,#11432,.T.);
#16199=ORIENTED_EDGE('',*,*,#11442,.T.);
#16200=ORIENTED_EDGE('',*,*,#11443,.T.);
#16201=ORIENTED_EDGE('',*,*,#11399,.T.);
#16202=ORIENTED_EDGE('',*,*,#10238,.T.);
#16203=ORIENTED_EDGE('',*,*,#11564,.F.);
#16204=ORIENTED_EDGE('',*,*,#11565,.F.);
#16205=ORIENTED_EDGE('',*,*,#11466,.T.);
#16206=ORIENTED_EDGE('',*,*,#10245,.T.);
#16207=ORIENTED_EDGE('',*,*,#11566,.F.);
#16208=ORIENTED_EDGE('',*,*,#11567,.F.);
#16209=ORIENTED_EDGE('',*,*,#11568,.F.);
#16210=ORIENTED_EDGE('',*,*,#10210,.T.);
#16211=ORIENTED_EDGE('',*,*,#11433,.T.);
#16212=ORIENTED_EDGE('',*,*,#11434,.T.);
#16213=ORIENTED_EDGE('',*,*,#11437,.T.);
#16214=ORIENTED_EDGE('',*,*,#11438,.T.);
#16215=ORIENTED_EDGE('',*,*,#11365,.T.);
#16216=ORIENTED_EDGE('',*,*,#10281,.T.);
#16217=ORIENTED_EDGE('',*,*,#11368,.T.);
#16218=ORIENTED_EDGE('',*,*,#11439,.T.);
#16219=ORIENTED_EDGE('',*,*,#11569,.F.);
#16220=ORIENTED_EDGE('',*,*,#11570,.F.);
#16221=ORIENTED_EDGE('',*,*,#11566,.T.);
#16222=ORIENTED_EDGE('',*,*,#10244,.T.);
#16223=ORIENTED_EDGE('',*,*,#10240,.T.);
#16224=ORIENTED_EDGE('',*,*,#11571,.F.);
#16225=ORIENTED_EDGE('',*,*,#11572,.F.);
#16226=ORIENTED_EDGE('',*,*,#11573,.F.);
#16227=ORIENTED_EDGE('',*,*,#11569,.T.);
#16228=ORIENTED_EDGE('',*,*,#11574,.F.);
#16229=ORIENTED_EDGE('',*,*,#11575,.F.);
#16230=ORIENTED_EDGE('',*,*,#11572,.T.);
#16231=ORIENTED_EDGE('',*,*,#11571,.T.);
#16232=ORIENTED_EDGE('',*,*,#10239,.T.);
#16233=ORIENTED_EDGE('',*,*,#11576,.F.);
#16234=ORIENTED_EDGE('',*,*,#11454,.T.);
#16235=ORIENTED_EDGE('',*,*,#11455,.T.);
#16236=ORIENTED_EDGE('',*,*,#11445,.T.);
#16237=ORIENTED_EDGE('',*,*,#11448,.T.);
#16238=ORIENTED_EDGE('',*,*,#11450,.T.);
#16239=ORIENTED_EDGE('',*,*,#11452,.T.);
#16240=ORIENTED_EDGE('',*,*,#11577,.F.);
#16241=ORIENTED_EDGE('',*,*,#11578,.F.);
#16242=ORIENTED_EDGE('',*,*,#11574,.T.);
#16243=ORIENTED_EDGE('',*,*,#10199,.T.);
#16244=ORIENTED_EDGE('',*,*,#11579,.F.);
#16245=ORIENTED_EDGE('',*,*,#11577,.T.);
#16246=ORIENTED_EDGE('',*,*,#11576,.T.);
#16247=ORIENTED_EDGE('',*,*,#10243,.T.);
#16248=ORIENTED_EDGE('',*,*,#10196,.T.);
#16249=ORIENTED_EDGE('',*,*,#11580,.F.);
#16250=ORIENTED_EDGE('',*,*,#11581,.F.);
#16251=ORIENTED_EDGE('',*,*,#10205,.T.);
#16252=ORIENTED_EDGE('',*,*,#11582,.F.);
#16253=ORIENTED_EDGE('',*,*,#11583,.F.);
#16254=ORIENTED_EDGE('',*,*,#10192,.T.);
#16255=ORIENTED_EDGE('',*,*,#11584,.F.);
#16256=ORIENTED_EDGE('',*,*,#11585,.F.);
#16257=ORIENTED_EDGE('',*,*,#10198,.T.);
#16258=ORIENTED_EDGE('',*,*,#11586,.F.);
#16259=ORIENTED_EDGE('',*,*,#11587,.F.);
#16260=ORIENTED_EDGE('',*,*,#10194,.T.);
#16261=ORIENTED_EDGE('',*,*,#11588,.F.);
#16262=ORIENTED_EDGE('',*,*,#11589,.T.);
#16263=ORIENTED_EDGE('',*,*,#11590,.F.);
#16264=ORIENTED_EDGE('',*,*,#11524,.F.);
#16265=ORIENTED_EDGE('',*,*,#11591,.F.);
#16266=ORIENTED_EDGE('',*,*,#11541,.F.);
#16267=ORIENTED_EDGE('',*,*,#11538,.F.);
#16268=ORIENTED_EDGE('',*,*,#11592,.F.);
#16269=ORIENTED_EDGE('',*,*,#11589,.F.);
#16270=ORIENTED_EDGE('',*,*,#11593,.F.);
#16271=ORIENTED_EDGE('',*,*,#11519,.F.);
#16272=ORIENTED_EDGE('',*,*,#11594,.F.);
#16273=ORIENTED_EDGE('',*,*,#11595,.F.);
#16274=ORIENTED_EDGE('',*,*,#11537,.T.);
#16275=ORIENTED_EDGE('',*,*,#11596,.F.);
#16276=ORIENTED_EDGE('',*,*,#11597,.F.);
#16277=ORIENTED_EDGE('',*,*,#11598,.T.);
#16278=ORIENTED_EDGE('',*,*,#11599,.F.);
#16279=ORIENTED_EDGE('',*,*,#11600,.F.);
#16280=ORIENTED_EDGE('',*,*,#11601,.F.);
#16281=ORIENTED_EDGE('',*,*,#11602,.T.);
#16282=ORIENTED_EDGE('',*,*,#11603,.F.);
#16283=ORIENTED_EDGE('',*,*,#11557,.F.);
#16284=ORIENTED_EDGE('',*,*,#11604,.F.);
#16285=ORIENTED_EDGE('',*,*,#11605,.T.);
#16286=ORIENTED_EDGE('',*,*,#11606,.F.);
#16287=ORIENTED_EDGE('',*,*,#11607,.F.);
#16288=ORIENTED_EDGE('',*,*,#11608,.T.);
#16289=ORIENTED_EDGE('',*,*,#11608,.F.);
#16290=ORIENTED_EDGE('',*,*,#11602,.F.);
#16291=ORIENTED_EDGE('',*,*,#11609,.F.);
#16292=ORIENTED_EDGE('',*,*,#11610,.F.);
#16293=ORIENTED_EDGE('',*,*,#11609,.T.);
#16294=ORIENTED_EDGE('',*,*,#11601,.T.);
#16295=ORIENTED_EDGE('',*,*,#11611,.F.);
#16296=ORIENTED_EDGE('',*,*,#11612,.T.);
#16297=ORIENTED_EDGE('',*,*,#11613,.F.);
#16298=ORIENTED_EDGE('',*,*,#11583,.T.);
#16299=ORIENTED_EDGE('',*,*,#11582,.T.);
#16300=ORIENTED_EDGE('',*,*,#10204,.T.);
#16301=ORIENTED_EDGE('',*,*,#11456,.T.);
#16302=ORIENTED_EDGE('',*,*,#11460,.T.);
#16303=ORIENTED_EDGE('',*,*,#11463,.T.);
#16304=ORIENTED_EDGE('',*,*,#11465,.T.);
#16305=ORIENTED_EDGE('',*,*,#11467,.T.);
#16306=ORIENTED_EDGE('',*,*,#11565,.T.);
#16307=ORIENTED_EDGE('',*,*,#11564,.T.);
#16308=ORIENTED_EDGE('',*,*,#10237,.T.);
#16309=ORIENTED_EDGE('',*,*,#11563,.T.);
#16310=ORIENTED_EDGE('',*,*,#11562,.T.);
#16311=ORIENTED_EDGE('',*,*,#10213,.T.);
#16312=ORIENTED_EDGE('',*,*,#11558,.T.);
#16313=ORIENTED_EDGE('',*,*,#11603,.T.);
#16314=ORIENTED_EDGE('',*,*,#11607,.T.);
#16315=ORIENTED_EDGE('',*,*,#11614,.F.);
#16316=ORIENTED_EDGE('',*,*,#11615,.F.);
#16317=ORIENTED_EDGE('',*,*,#11616,.F.);
#16318=ORIENTED_EDGE('',*,*,#11596,.T.);
#16319=ORIENTED_EDGE('',*,*,#11617,.T.);
#16320=ORIENTED_EDGE('',*,*,#11516,.T.);
#16321=ORIENTED_EDGE('',*,*,#11593,.T.);
#16322=ORIENTED_EDGE('',*,*,#11588,.T.);
#16323=ORIENTED_EDGE('',*,*,#10193,.T.);
#16324=ORIENTED_EDGE('',*,*,#11587,.T.);
#16325=ORIENTED_EDGE('',*,*,#11586,.T.);
#16326=ORIENTED_EDGE('',*,*,#10197,.T.);
#16327=ORIENTED_EDGE('',*,*,#11618,.T.);
#16328=ORIENTED_EDGE('',*,*,#11619,.F.);
#16329=ORIENTED_EDGE('',*,*,#11620,.T.);
#16330=ORIENTED_EDGE('',*,*,#11472,.F.);
#16331=ORIENTED_EDGE('',*,*,#11621,.T.);
#16332=ORIENTED_EDGE('',*,*,#11622,.F.);
#16333=ORIENTED_EDGE('',*,*,#11618,.F.);
#16334=ORIENTED_EDGE('',*,*,#11471,.F.);
#16335=ORIENTED_EDGE('',*,*,#11623,.T.);
#16336=ORIENTED_EDGE('',*,*,#11624,.F.);
#16337=ORIENTED_EDGE('',*,*,#11621,.F.);
#16338=ORIENTED_EDGE('',*,*,#11470,.F.);
#16339=ORIENTED_EDGE('',*,*,#11625,.T.);
#16340=ORIENTED_EDGE('',*,*,#11626,.F.);
#16341=ORIENTED_EDGE('',*,*,#11623,.F.);
#16342=ORIENTED_EDGE('',*,*,#11469,.F.);
#16343=ORIENTED_EDGE('',*,*,#11627,.T.);
#16344=ORIENTED_EDGE('',*,*,#11628,.F.);
#16345=ORIENTED_EDGE('',*,*,#11625,.F.);
#16346=ORIENTED_EDGE('',*,*,#11468,.F.);
#16347=ORIENTED_EDGE('',*,*,#11620,.F.);
#16348=ORIENTED_EDGE('',*,*,#11629,.F.);
#16349=ORIENTED_EDGE('',*,*,#11627,.F.);
#16350=ORIENTED_EDGE('',*,*,#11473,.F.);
#16351=ORIENTED_EDGE('',*,*,#11630,.F.);
#16352=ORIENTED_EDGE('',*,*,#11631,.F.);
#16353=ORIENTED_EDGE('',*,*,#11615,.T.);
#16354=ORIENTED_EDGE('',*,*,#11632,.T.);
#16355=ORIENTED_EDGE('',*,*,#11633,.F.);
#16356=ORIENTED_EDGE('',*,*,#11634,.T.);
#16357=ORIENTED_EDGE('',*,*,#11635,.F.);
#16358=ORIENTED_EDGE('',*,*,#11605,.F.);
#16359=ORIENTED_EDGE('',*,*,#11632,.F.);
#16360=ORIENTED_EDGE('',*,*,#11636,.T.);
#16361=ORIENTED_EDGE('',*,*,#11637,.T.);
#16362=ORIENTED_EDGE('',*,*,#11638,.T.);
#16363=ORIENTED_EDGE('',*,*,#11639,.F.);
#16364=ORIENTED_EDGE('',*,*,#11599,.T.);
#16365=ORIENTED_EDGE('',*,*,#11635,.T.);
#16366=ORIENTED_EDGE('',*,*,#11640,.T.);
#16367=ORIENTED_EDGE('',*,*,#11641,.T.);
#16368=ORIENTED_EDGE('',*,*,#11642,.T.);
#16369=ORIENTED_EDGE('',*,*,#11478,.F.);
#16370=ORIENTED_EDGE('',*,*,#11642,.F.);
#16371=ORIENTED_EDGE('',*,*,#11643,.T.);
#16372=ORIENTED_EDGE('',*,*,#11644,.T.);
#16373=ORIENTED_EDGE('',*,*,#11479,.F.);
#16374=ORIENTED_EDGE('',*,*,#11644,.F.);
#16375=ORIENTED_EDGE('',*,*,#11645,.T.);
#16376=ORIENTED_EDGE('',*,*,#11646,.T.);
#16377=ORIENTED_EDGE('',*,*,#11474,.F.);
#16378=ORIENTED_EDGE('',*,*,#11646,.F.);
#16379=ORIENTED_EDGE('',*,*,#11647,.T.);
#16380=ORIENTED_EDGE('',*,*,#11648,.T.);
#16381=ORIENTED_EDGE('',*,*,#11475,.F.);
#16382=ORIENTED_EDGE('',*,*,#11648,.F.);
#16383=ORIENTED_EDGE('',*,*,#11649,.T.);
#16384=ORIENTED_EDGE('',*,*,#11650,.T.);
#16385=ORIENTED_EDGE('',*,*,#11476,.F.);
#16386=ORIENTED_EDGE('',*,*,#11650,.F.);
#16387=ORIENTED_EDGE('',*,*,#11651,.T.);
#16388=ORIENTED_EDGE('',*,*,#11640,.F.);
#16389=ORIENTED_EDGE('',*,*,#11477,.F.);
#16390=ORIENTED_EDGE('',*,*,#11652,.T.);
#16391=ORIENTED_EDGE('',*,*,#11482,.F.);
#16392=ORIENTED_EDGE('',*,*,#11653,.T.);
#16393=ORIENTED_EDGE('',*,*,#11654,.F.);
#16394=ORIENTED_EDGE('',*,*,#11653,.F.);
#16395=ORIENTED_EDGE('',*,*,#11481,.F.);
#16396=ORIENTED_EDGE('',*,*,#11655,.T.);
#16397=ORIENTED_EDGE('',*,*,#11656,.F.);
#16398=ORIENTED_EDGE('',*,*,#11655,.F.);
#16399=ORIENTED_EDGE('',*,*,#11480,.F.);
#16400=ORIENTED_EDGE('',*,*,#11657,.T.);
#16401=ORIENTED_EDGE('',*,*,#11658,.F.);
#16402=ORIENTED_EDGE('',*,*,#11657,.F.);
#16403=ORIENTED_EDGE('',*,*,#11485,.F.);
#16404=ORIENTED_EDGE('',*,*,#11659,.T.);
#16405=ORIENTED_EDGE('',*,*,#11660,.F.);
#16406=ORIENTED_EDGE('',*,*,#11659,.F.);
#16407=ORIENTED_EDGE('',*,*,#11484,.F.);
#16408=ORIENTED_EDGE('',*,*,#11661,.T.);
#16409=ORIENTED_EDGE('',*,*,#11662,.F.);
#16410=ORIENTED_EDGE('',*,*,#11661,.F.);
#16411=ORIENTED_EDGE('',*,*,#11483,.F.);
#16412=ORIENTED_EDGE('',*,*,#11652,.F.);
#16413=ORIENTED_EDGE('',*,*,#11663,.F.);
#16414=ORIENTED_EDGE('',*,*,#10190,.F.);
#16415=ORIENTED_EDGE('',*,*,#10232,.T.);
#16416=ORIENTED_EDGE('',*,*,#11664,.T.);
#16417=ORIENTED_EDGE('',*,*,#11665,.T.);
#16418=ORIENTED_EDGE('',*,*,#11666,.T.);
#16419=ORIENTED_EDGE('',*,*,#11667,.T.);
#16420=ORIENTED_EDGE('',*,*,#11668,.T.);
#16421=ORIENTED_EDGE('',*,*,#11669,.T.);
#16422=ORIENTED_EDGE('',*,*,#10185,.F.);
#16423=ORIENTED_EDGE('',*,*,#11488,.F.);
#16424=ORIENTED_EDGE('',*,*,#11486,.F.);
#16425=ORIENTED_EDGE('',*,*,#10218,.F.);
#16426=ORIENTED_EDGE('',*,*,#11490,.F.);
#16427=ORIENTED_EDGE('',*,*,#10220,.F.);
#16428=ORIENTED_EDGE('',*,*,#10223,.F.);
#16429=ORIENTED_EDGE('',*,*,#10226,.F.);
#16430=ORIENTED_EDGE('',*,*,#10229,.F.);
#16431=ORIENTED_EDGE('',*,*,#11670,.F.);
#16432=ORIENTED_EDGE('',*,*,#11671,.F.);
#16433=ORIENTED_EDGE('',*,*,#11672,.F.);
#16434=ORIENTED_EDGE('',*,*,#11673,.F.);
#16435=ORIENTED_EDGE('',*,*,#11674,.F.);
#16436=ORIENTED_EDGE('',*,*,#11675,.F.);
#16437=ORIENTED_EDGE('',*,*,#11676,.T.);
#16438=ORIENTED_EDGE('',*,*,#11677,.F.);
#16439=ORIENTED_EDGE('',*,*,#11670,.T.);
#16440=ORIENTED_EDGE('',*,*,#11678,.F.);
#16441=ORIENTED_EDGE('',*,*,#11679,.F.);
#16442=ORIENTED_EDGE('',*,*,#11676,.F.);
#16443=ORIENTED_EDGE('',*,*,#11680,.F.);
#16444=ORIENTED_EDGE('',*,*,#11681,.F.);
#16445=ORIENTED_EDGE('',*,*,#11682,.F.);
#16446=ORIENTED_EDGE('',*,*,#11683,.F.);
#16447=ORIENTED_EDGE('',*,*,#11684,.T.);
#16448=ORIENTED_EDGE('',*,*,#11685,.F.);
#16449=ORIENTED_EDGE('',*,*,#11682,.T.);
#16450=ORIENTED_EDGE('',*,*,#11686,.F.);
#16451=ORIENTED_EDGE('',*,*,#11687,.T.);
#16452=ORIENTED_EDGE('',*,*,#11496,.F.);
#16453=ORIENTED_EDGE('',*,*,#11688,.T.);
#16454=ORIENTED_EDGE('',*,*,#11689,.F.);
#16455=ORIENTED_EDGE('',*,*,#11688,.F.);
#16456=ORIENTED_EDGE('',*,*,#11495,.F.);
#16457=ORIENTED_EDGE('',*,*,#11690,.T.);
#16458=ORIENTED_EDGE('',*,*,#11691,.F.);
#16459=ORIENTED_EDGE('',*,*,#11690,.F.);
#16460=ORIENTED_EDGE('',*,*,#11494,.F.);
#16461=ORIENTED_EDGE('',*,*,#11692,.T.);
#16462=ORIENTED_EDGE('',*,*,#11693,.F.);
#16463=ORIENTED_EDGE('',*,*,#11692,.F.);
#16464=ORIENTED_EDGE('',*,*,#11493,.F.);
#16465=ORIENTED_EDGE('',*,*,#11694,.T.);
#16466=ORIENTED_EDGE('',*,*,#11695,.F.);
#16467=ORIENTED_EDGE('',*,*,#11694,.F.);
#16468=ORIENTED_EDGE('',*,*,#11492,.F.);
#16469=ORIENTED_EDGE('',*,*,#11696,.T.);
#16470=ORIENTED_EDGE('',*,*,#11697,.F.);
#16471=ORIENTED_EDGE('',*,*,#11696,.F.);
#16472=ORIENTED_EDGE('',*,*,#11491,.F.);
#16473=ORIENTED_EDGE('',*,*,#11687,.F.);
#16474=ORIENTED_EDGE('',*,*,#11698,.F.);
#16475=ORIENTED_EDGE('',*,*,#11699,.F.);
#16476=ORIENTED_EDGE('',*,*,#11700,.F.);
#16477=ORIENTED_EDGE('',*,*,#11701,.T.);
#16478=ORIENTED_EDGE('',*,*,#11502,.F.);
#16479=ORIENTED_EDGE('',*,*,#11702,.T.);
#16480=ORIENTED_EDGE('',*,*,#11703,.F.);
#16481=ORIENTED_EDGE('',*,*,#11702,.F.);
#16482=ORIENTED_EDGE('',*,*,#11501,.F.);
#16483=ORIENTED_EDGE('',*,*,#11704,.T.);
#16484=ORIENTED_EDGE('',*,*,#11705,.F.);
#16485=ORIENTED_EDGE('',*,*,#11704,.F.);
#16486=ORIENTED_EDGE('',*,*,#11500,.F.);
#16487=ORIENTED_EDGE('',*,*,#11706,.T.);
#16488=ORIENTED_EDGE('',*,*,#11707,.F.);
#16489=ORIENTED_EDGE('',*,*,#11706,.F.);
#16490=ORIENTED_EDGE('',*,*,#11499,.F.);
#16491=ORIENTED_EDGE('',*,*,#11708,.T.);
#16492=ORIENTED_EDGE('',*,*,#11709,.F.);
#16493=ORIENTED_EDGE('',*,*,#11710,.F.);
#16494=ORIENTED_EDGE('',*,*,#11711,.F.);
#16495=ORIENTED_EDGE('',*,*,#11708,.F.);
#16496=ORIENTED_EDGE('',*,*,#11498,.F.);
#16497=ORIENTED_EDGE('',*,*,#11712,.T.);
#16498=ORIENTED_EDGE('',*,*,#11713,.F.);
#16499=ORIENTED_EDGE('',*,*,#11712,.F.);
#16500=ORIENTED_EDGE('',*,*,#11497,.F.);
#16501=ORIENTED_EDGE('',*,*,#11701,.F.);
#16502=ORIENTED_EDGE('',*,*,#11714,.F.);
#16503=ORIENTED_EDGE('',*,*,#10182,.F.);
#16504=ORIENTED_EDGE('',*,*,#11513,.T.);
#16505=ORIENTED_EDGE('',*,*,#11514,.T.);
#16506=ORIENTED_EDGE('',*,*,#11505,.T.);
#16507=ORIENTED_EDGE('',*,*,#11507,.T.);
#16508=ORIENTED_EDGE('',*,*,#11509,.T.);
#16509=ORIENTED_EDGE('',*,*,#11511,.T.);
#16510=ORIENTED_EDGE('',*,*,#11542,.T.);
#16511=ORIENTED_EDGE('',*,*,#11591,.T.);
#16512=ORIENTED_EDGE('',*,*,#11523,.T.);
#16513=ORIENTED_EDGE('',*,*,#11715,.T.);
#16514=ORIENTED_EDGE('',*,*,#11598,.F.);
#16515=ORIENTED_EDGE('',*,*,#11716,.F.);
#16516=ORIENTED_EDGE('',*,*,#11717,.T.);
#16517=ORIENTED_EDGE('',*,*,#11521,.F.);
#16518=ORIENTED_EDGE('',*,*,#11520,.F.);
#16519=ORIENTED_EDGE('',*,*,#11517,.F.);
#16520=ORIENTED_EDGE('',*,*,#11617,.F.);
#16521=ORIENTED_EDGE('',*,*,#11534,.F.);
#16522=ORIENTED_EDGE('',*,*,#11532,.F.);
#16523=ORIENTED_EDGE('',*,*,#11530,.F.);
#16524=ORIENTED_EDGE('',*,*,#11528,.F.);
#16525=ORIENTED_EDGE('',*,*,#11526,.F.);
#16526=ORIENTED_EDGE('',*,*,#11536,.F.);
#16527=ORIENTED_EDGE('',*,*,#11718,.F.);
#16528=ORIENTED_EDGE('',*,*,#11719,.F.);
#16529=ORIENTED_EDGE('',*,*,#11720,.F.);
#16530=ORIENTED_EDGE('',*,*,#11718,.T.);
#16531=ORIENTED_EDGE('',*,*,#11721,.F.);
#16532=ORIENTED_EDGE('',*,*,#11594,.T.);
#16533=ORIENTED_EDGE('',*,*,#11540,.T.);
#16534=ORIENTED_EDGE('',*,*,#11544,.T.);
#16535=ORIENTED_EDGE('',*,*,#11722,.T.);
#16536=ORIENTED_EDGE('',*,*,#11723,.F.);
#16537=ORIENTED_EDGE('',*,*,#11555,.T.);
#16538=ORIENTED_EDGE('',*,*,#11556,.T.);
#16539=ORIENTED_EDGE('',*,*,#11546,.T.);
#16540=ORIENTED_EDGE('',*,*,#11549,.T.);
#16541=ORIENTED_EDGE('',*,*,#11551,.T.);
#16542=ORIENTED_EDGE('',*,*,#11553,.T.);
#16543=ORIENTED_EDGE('',*,*,#11724,.T.);
#16544=ORIENTED_EDGE('',*,*,#11725,.F.);
#16545=ORIENTED_EDGE('',*,*,#11726,.T.);
#16546=ORIENTED_EDGE('',*,*,#11633,.T.);
#16547=ORIENTED_EDGE('',*,*,#11604,.T.);
#16548=ORIENTED_EDGE('',*,*,#11559,.T.);
#16549=ORIENTED_EDGE('',*,*,#10211,.T.);
#16550=ORIENTED_EDGE('',*,*,#11561,.T.);
#16551=ORIENTED_EDGE('',*,*,#11560,.T.);
#16552=ORIENTED_EDGE('',*,*,#10207,.T.);
#16553=ORIENTED_EDGE('',*,*,#11568,.T.);
#16554=ORIENTED_EDGE('',*,*,#11567,.T.);
#16555=ORIENTED_EDGE('',*,*,#11570,.T.);
#16556=ORIENTED_EDGE('',*,*,#11573,.T.);
#16557=ORIENTED_EDGE('',*,*,#11575,.T.);
#16558=ORIENTED_EDGE('',*,*,#11578,.T.);
#16559=ORIENTED_EDGE('',*,*,#11579,.T.);
#16560=ORIENTED_EDGE('',*,*,#10206,.T.);
#16561=ORIENTED_EDGE('',*,*,#11581,.T.);
#16562=ORIENTED_EDGE('',*,*,#11580,.T.);
#16563=ORIENTED_EDGE('',*,*,#10195,.T.);
#16564=ORIENTED_EDGE('',*,*,#11585,.T.);
#16565=ORIENTED_EDGE('',*,*,#11584,.T.);
#16566=ORIENTED_EDGE('',*,*,#10191,.T.);
#16567=ORIENTED_EDGE('',*,*,#11590,.T.);
#16568=ORIENTED_EDGE('',*,*,#11592,.T.);
#16569=ORIENTED_EDGE('',*,*,#11595,.T.);
#16570=ORIENTED_EDGE('',*,*,#11721,.T.);
#16571=ORIENTED_EDGE('',*,*,#11720,.T.);
#16572=ORIENTED_EDGE('',*,*,#11725,.T.);
#16573=ORIENTED_EDGE('',*,*,#11727,.F.);
#16574=ORIENTED_EDGE('',*,*,#11728,.T.);
#16575=ORIENTED_EDGE('',*,*,#11729,.F.);
#16576=ORIENTED_EDGE('',*,*,#11684,.F.);
#16577=ORIENTED_EDGE('',*,*,#11730,.F.);
#16578=ORIENTED_EDGE('',*,*,#11731,.F.);
#16579=ORIENTED_EDGE('',*,*,#11732,.F.);
#16580=ORIENTED_EDGE('',*,*,#11733,.T.);
#16581=ORIENTED_EDGE('',*,*,#11716,.T.);
#16582=ORIENTED_EDGE('',*,*,#11597,.T.);
#16583=ORIENTED_EDGE('',*,*,#11734,.F.);
#16584=ORIENTED_EDGE('',*,*,#11735,.F.);
#16585=ORIENTED_EDGE('',*,*,#11734,.T.);
#16586=ORIENTED_EDGE('',*,*,#11616,.T.);
#16587=ORIENTED_EDGE('',*,*,#11736,.F.);
#16588=ORIENTED_EDGE('',*,*,#11611,.T.);
#16589=ORIENTED_EDGE('',*,*,#11600,.T.);
#16590=ORIENTED_EDGE('',*,*,#11639,.T.);
#16591=ORIENTED_EDGE('',*,*,#11737,.T.);
#16592=ORIENTED_EDGE('',*,*,#11630,.T.);
#16593=ORIENTED_EDGE('',*,*,#11614,.T.);
#16594=ORIENTED_EDGE('',*,*,#11606,.T.);
#16595=ORIENTED_EDGE('',*,*,#11610,.T.);
#16596=ORIENTED_EDGE('',*,*,#11613,.T.);
#16597=ORIENTED_EDGE('',*,*,#11738,.T.);
#16598=ORIENTED_EDGE('',*,*,#11739,.F.);
#16599=ORIENTED_EDGE('',*,*,#11628,.T.);
#16600=ORIENTED_EDGE('',*,*,#11629,.T.);
#16601=ORIENTED_EDGE('',*,*,#11619,.T.);
#16602=ORIENTED_EDGE('',*,*,#11622,.T.);
#16603=ORIENTED_EDGE('',*,*,#11624,.T.);
#16604=ORIENTED_EDGE('',*,*,#11626,.T.);
#16605=ORIENTED_EDGE('',*,*,#11740,.F.);
#16606=ORIENTED_EDGE('',*,*,#11736,.T.);
#16607=ORIENTED_EDGE('',*,*,#11631,.T.);
#16608=ORIENTED_EDGE('',*,*,#11739,.T.);
#16609=ORIENTED_EDGE('',*,*,#11741,.T.);
#16610=ORIENTED_EDGE('',*,*,#11728,.F.);
#16611=ORIENTED_EDGE('',*,*,#11742,.F.);
#16612=ORIENTED_EDGE('',*,*,#11743,.T.);
#16613=ORIENTED_EDGE('',*,*,#11637,.F.);
#16614=ORIENTED_EDGE('',*,*,#11636,.F.);
#16615=ORIENTED_EDGE('',*,*,#11634,.F.);
#16616=ORIENTED_EDGE('',*,*,#11726,.F.);
#16617=ORIENTED_EDGE('',*,*,#11649,.F.);
#16618=ORIENTED_EDGE('',*,*,#11647,.F.);
#16619=ORIENTED_EDGE('',*,*,#11645,.F.);
#16620=ORIENTED_EDGE('',*,*,#11643,.F.);
#16621=ORIENTED_EDGE('',*,*,#11641,.F.);
#16622=ORIENTED_EDGE('',*,*,#11651,.F.);
#16623=ORIENTED_EDGE('',*,*,#10169,.F.);
#16624=ORIENTED_EDGE('',*,*,#11662,.T.);
#16625=ORIENTED_EDGE('',*,*,#11663,.T.);
#16626=ORIENTED_EDGE('',*,*,#11654,.T.);
#16627=ORIENTED_EDGE('',*,*,#11656,.T.);
#16628=ORIENTED_EDGE('',*,*,#11658,.T.);
#16629=ORIENTED_EDGE('',*,*,#11660,.T.);
#16630=ORIENTED_EDGE('',*,*,#11744,.T.);
#16631=ORIENTED_EDGE('',*,*,#11669,.F.);
#16632=ORIENTED_EDGE('',*,*,#11745,.T.);
#16633=ORIENTED_EDGE('',*,*,#11746,.F.);
#16634=ORIENTED_EDGE('',*,*,#11745,.F.);
#16635=ORIENTED_EDGE('',*,*,#11668,.F.);
#16636=ORIENTED_EDGE('',*,*,#11747,.T.);
#16637=ORIENTED_EDGE('',*,*,#11748,.F.);
#16638=ORIENTED_EDGE('',*,*,#11747,.F.);
#16639=ORIENTED_EDGE('',*,*,#11667,.F.);
#16640=ORIENTED_EDGE('',*,*,#11749,.T.);
#16641=ORIENTED_EDGE('',*,*,#11750,.F.);
#16642=ORIENTED_EDGE('',*,*,#11749,.F.);
#16643=ORIENTED_EDGE('',*,*,#11666,.F.);
#16644=ORIENTED_EDGE('',*,*,#11751,.T.);
#16645=ORIENTED_EDGE('',*,*,#11752,.F.);
#16646=ORIENTED_EDGE('',*,*,#11751,.F.);
#16647=ORIENTED_EDGE('',*,*,#11665,.F.);
#16648=ORIENTED_EDGE('',*,*,#11753,.T.);
#16649=ORIENTED_EDGE('',*,*,#11754,.F.);
#16650=ORIENTED_EDGE('',*,*,#11753,.F.);
#16651=ORIENTED_EDGE('',*,*,#11664,.F.);
#16652=ORIENTED_EDGE('',*,*,#11744,.F.);
#16653=ORIENTED_EDGE('',*,*,#11755,.F.);
#16654=ORIENTED_EDGE('',*,*,#11730,.T.);
#16655=ORIENTED_EDGE('',*,*,#11686,.T.);
#16656=ORIENTED_EDGE('',*,*,#11681,.T.);
#16657=ORIENTED_EDGE('',*,*,#11756,.F.);
#16658=ORIENTED_EDGE('',*,*,#11680,.T.);
#16659=ORIENTED_EDGE('',*,*,#11678,.T.);
#16660=ORIENTED_EDGE('',*,*,#11675,.T.);
#16661=ORIENTED_EDGE('',*,*,#11757,.F.);
#16662=ORIENTED_EDGE('',*,*,#11758,.F.);
#16663=ORIENTED_EDGE('',*,*,#11759,.F.);
#16664=ORIENTED_EDGE('',*,*,#11674,.T.);
#16665=ORIENTED_EDGE('',*,*,#11760,.F.);
#16666=ORIENTED_EDGE('',*,*,#11761,.F.);
#16667=ORIENTED_EDGE('',*,*,#11760,.T.);
#16668=ORIENTED_EDGE('',*,*,#11673,.T.);
#16669=ORIENTED_EDGE('',*,*,#11762,.F.);
#16670=ORIENTED_EDGE('',*,*,#11763,.F.);
#16671=ORIENTED_EDGE('',*,*,#11762,.T.);
#16672=ORIENTED_EDGE('',*,*,#11672,.T.);
#16673=ORIENTED_EDGE('',*,*,#11764,.F.);
#16674=ORIENTED_EDGE('',*,*,#11679,.T.);
#16675=ORIENTED_EDGE('',*,*,#11765,.F.);
#16676=ORIENTED_EDGE('',*,*,#11671,.T.);
#16677=ORIENTED_EDGE('',*,*,#11677,.T.);
#16678=ORIENTED_EDGE('',*,*,#11729,.T.);
#16679=ORIENTED_EDGE('',*,*,#11766,.F.);
#16680=ORIENTED_EDGE('',*,*,#11683,.T.);
#16681=ORIENTED_EDGE('',*,*,#11685,.T.);
#16682=ORIENTED_EDGE('',*,*,#10168,.F.);
#16683=ORIENTED_EDGE('',*,*,#11697,.T.);
#16684=ORIENTED_EDGE('',*,*,#11698,.T.);
#16685=ORIENTED_EDGE('',*,*,#11689,.T.);
#16686=ORIENTED_EDGE('',*,*,#11691,.T.);
#16687=ORIENTED_EDGE('',*,*,#11693,.T.);
#16688=ORIENTED_EDGE('',*,*,#11695,.T.);
#16689=ORIENTED_EDGE('',*,*,#11711,.T.);
#16690=ORIENTED_EDGE('',*,*,#11767,.T.);
#16691=ORIENTED_EDGE('',*,*,#11703,.T.);
#16692=ORIENTED_EDGE('',*,*,#11705,.T.);
#16693=ORIENTED_EDGE('',*,*,#11707,.T.);
#16694=ORIENTED_EDGE('',*,*,#11714,.T.);
#16695=ORIENTED_EDGE('',*,*,#11700,.T.);
#16696=ORIENTED_EDGE('',*,*,#11768,.T.);
#16697=ORIENTED_EDGE('',*,*,#10174,.T.);
#16698=ORIENTED_EDGE('',*,*,#11769,.T.);
#16699=ORIENTED_EDGE('',*,*,#11709,.T.);
#16700=ORIENTED_EDGE('',*,*,#11713,.T.);
#16701=ORIENTED_EDGE('',*,*,#11770,.F.);
#16702=ORIENTED_EDGE('',*,*,#11771,.T.);
#16703=ORIENTED_EDGE('',*,*,#11772,.F.);
#16704=ORIENTED_EDGE('',*,*,#11773,.T.);
#16705=ORIENTED_EDGE('',*,*,#11774,.F.);
#16706=ORIENTED_EDGE('',*,*,#10183,.F.);
#16707=ORIENTED_EDGE('',*,*,#10180,.F.);
#16708=ORIENTED_EDGE('',*,*,#11717,.F.);
#16709=ORIENTED_EDGE('',*,*,#11733,.F.);
#16710=ORIENTED_EDGE('',*,*,#11775,.F.);
#16711=ORIENTED_EDGE('',*,*,#11776,.F.);
#16712=ORIENTED_EDGE('',*,*,#11722,.F.);
#16713=ORIENTED_EDGE('',*,*,#11543,.F.);
#16714=ORIENTED_EDGE('',*,*,#11715,.F.);
#16715=ORIENTED_EDGE('',*,*,#11522,.F.);
#16716=ORIENTED_EDGE('',*,*,#11777,.T.);
#16717=ORIENTED_EDGE('',*,*,#11778,.T.);
#16718=ORIENTED_EDGE('',*,*,#11719,.T.);
#16719=ORIENTED_EDGE('',*,*,#11723,.T.);
#16720=ORIENTED_EDGE('',*,*,#11776,.T.);
#16721=ORIENTED_EDGE('',*,*,#11779,.F.);
#16722=ORIENTED_EDGE('',*,*,#11780,.F.);
#16723=ORIENTED_EDGE('',*,*,#11724,.F.);
#16724=ORIENTED_EDGE('',*,*,#11778,.F.);
#16725=ORIENTED_EDGE('',*,*,#11781,.T.);
#16726=ORIENTED_EDGE('',*,*,#11782,.F.);
#16727=ORIENTED_EDGE('',*,*,#11783,.T.);
#16728=ORIENTED_EDGE('',*,*,#11742,.T.);
#16729=ORIENTED_EDGE('',*,*,#11727,.T.);
#16730=ORIENTED_EDGE('',*,*,#11780,.T.);
#16731=ORIENTED_EDGE('',*,*,#11784,.T.);
#16732=ORIENTED_EDGE('',*,*,#11732,.T.);
#16733=ORIENTED_EDGE('',*,*,#11735,.T.);
#16734=ORIENTED_EDGE('',*,*,#11740,.T.);
#16735=ORIENTED_EDGE('',*,*,#11785,.F.);
#16736=ORIENTED_EDGE('',*,*,#11731,.T.);
#16737=ORIENTED_EDGE('',*,*,#11786,.F.);
#16738=ORIENTED_EDGE('',*,*,#11743,.F.);
#16739=ORIENTED_EDGE('',*,*,#11783,.F.);
#16740=ORIENTED_EDGE('',*,*,#11787,.F.);
#16741=ORIENTED_EDGE('',*,*,#11741,.F.);
#16742=ORIENTED_EDGE('',*,*,#11738,.F.);
#16743=ORIENTED_EDGE('',*,*,#11612,.F.);
#16744=ORIENTED_EDGE('',*,*,#11737,.F.);
#16745=ORIENTED_EDGE('',*,*,#11638,.F.);
#16746=ORIENTED_EDGE('',*,*,#11788,.F.);
#16747=ORIENTED_EDGE('',*,*,#11789,.T.);
#16748=ORIENTED_EDGE('',*,*,#11790,.F.);
#16749=ORIENTED_EDGE('',*,*,#11791,.T.);
#16750=ORIENTED_EDGE('',*,*,#11792,.F.);
#16751=ORIENTED_EDGE('',*,*,#10163,.F.);
#16752=ORIENTED_EDGE('',*,*,#10158,.T.);
#16753=ORIENTED_EDGE('',*,*,#11793,.T.);
#16754=ORIENTED_EDGE('',*,*,#11794,.T.);
#16755=ORIENTED_EDGE('',*,*,#10162,.F.);
#16756=ORIENTED_EDGE('',*,*,#11795,.F.);
#16757=ORIENTED_EDGE('',*,*,#11796,.F.);
#16758=ORIENTED_EDGE('',*,*,#11797,.F.);
#16759=ORIENTED_EDGE('',*,*,#11798,.F.);
#16760=ORIENTED_EDGE('',*,*,#11799,.F.);
#16761=ORIENTED_EDGE('',*,*,#11800,.F.);
#16762=ORIENTED_EDGE('',*,*,#11801,.T.);
#16763=ORIENTED_EDGE('',*,*,#10156,.F.);
#16764=ORIENTED_EDGE('',*,*,#11794,.F.);
#16765=ORIENTED_EDGE('',*,*,#10188,.F.);
#16766=ORIENTED_EDGE('',*,*,#11801,.F.);
#16767=ORIENTED_EDGE('',*,*,#11802,.F.);
#16768=ORIENTED_EDGE('',*,*,#11793,.F.);
#16769=ORIENTED_EDGE('',*,*,#10157,.F.);
#16770=ORIENTED_EDGE('',*,*,#10161,.F.);
#16771=ORIENTED_EDGE('',*,*,#10152,.F.);
#16772=ORIENTED_EDGE('',*,*,#11803,.F.);
#16773=ORIENTED_EDGE('',*,*,#11795,.T.);
#16774=ORIENTED_EDGE('',*,*,#10150,.F.);
#16775=ORIENTED_EDGE('',*,*,#11754,.T.);
#16776=ORIENTED_EDGE('',*,*,#11755,.T.);
#16777=ORIENTED_EDGE('',*,*,#11746,.T.);
#16778=ORIENTED_EDGE('',*,*,#11748,.T.);
#16779=ORIENTED_EDGE('',*,*,#11750,.T.);
#16780=ORIENTED_EDGE('',*,*,#11752,.T.);
#16781=ORIENTED_EDGE('',*,*,#11804,.F.);
#16782=ORIENTED_EDGE('',*,*,#11805,.F.);
#16783=ORIENTED_EDGE('',*,*,#11806,.F.);
#16784=ORIENTED_EDGE('',*,*,#11807,.F.);
#16785=ORIENTED_EDGE('',*,*,#11808,.F.);
#16786=ORIENTED_EDGE('',*,*,#11809,.F.);
#16787=ORIENTED_EDGE('',*,*,#11806,.T.);
#16788=ORIENTED_EDGE('',*,*,#11756,.T.);
#16789=ORIENTED_EDGE('',*,*,#11810,.T.);
#16790=ORIENTED_EDGE('',*,*,#11811,.F.);
#16791=ORIENTED_EDGE('',*,*,#11812,.F.);
#16792=ORIENTED_EDGE('',*,*,#11813,.F.);
#16793=ORIENTED_EDGE('',*,*,#11814,.F.);
#16794=ORIENTED_EDGE('',*,*,#11810,.F.);
#16795=ORIENTED_EDGE('',*,*,#11812,.T.);
#16796=ORIENTED_EDGE('',*,*,#11757,.T.);
#16797=ORIENTED_EDGE('',*,*,#11815,.F.);
#16798=ORIENTED_EDGE('',*,*,#11816,.F.);
#16799=ORIENTED_EDGE('',*,*,#11817,.F.);
#16800=ORIENTED_EDGE('',*,*,#11815,.T.);
#16801=ORIENTED_EDGE('',*,*,#11818,.F.);
#16802=ORIENTED_EDGE('',*,*,#11819,.F.);
#16803=ORIENTED_EDGE('',*,*,#11820,.F.);
#16804=ORIENTED_EDGE('',*,*,#11821,.F.);
#16805=ORIENTED_EDGE('',*,*,#11818,.T.);
#16806=ORIENTED_EDGE('',*,*,#11759,.T.);
#16807=ORIENTED_EDGE('',*,*,#11822,.F.);
#16808=ORIENTED_EDGE('',*,*,#11823,.F.);
#16809=ORIENTED_EDGE('',*,*,#11824,.F.);
#16810=ORIENTED_EDGE('',*,*,#11825,.F.);
#16811=ORIENTED_EDGE('',*,*,#11826,.F.);
#16812=ORIENTED_EDGE('',*,*,#11827,.F.);
#16813=ORIENTED_EDGE('',*,*,#11820,.T.);
#16814=ORIENTED_EDGE('',*,*,#11758,.T.);
#16815=ORIENTED_EDGE('',*,*,#11761,.T.);
#16816=ORIENTED_EDGE('',*,*,#11763,.T.);
#16817=ORIENTED_EDGE('',*,*,#11828,.F.);
#16818=ORIENTED_EDGE('',*,*,#11829,.F.);
#16819=ORIENTED_EDGE('',*,*,#11830,.F.);
#16820=ORIENTED_EDGE('',*,*,#11831,.F.);
#16821=ORIENTED_EDGE('',*,*,#10187,.T.);
#16822=ORIENTED_EDGE('',*,*,#11828,.T.);
#16823=ORIENTED_EDGE('',*,*,#11764,.T.);
#16824=ORIENTED_EDGE('',*,*,#11832,.F.);
#16825=ORIENTED_EDGE('',*,*,#11833,.F.);
#16826=ORIENTED_EDGE('',*,*,#11834,.F.);
#16827=ORIENTED_EDGE('',*,*,#11835,.F.);
#16828=ORIENTED_EDGE('',*,*,#11832,.T.);
#16829=ORIENTED_EDGE('',*,*,#11836,.F.);
#16830=ORIENTED_EDGE('',*,*,#11837,.T.);
#16831=ORIENTED_EDGE('',*,*,#11838,.F.);
#16832=ORIENTED_EDGE('',*,*,#11836,.T.);
#16833=ORIENTED_EDGE('',*,*,#11765,.T.);
#16834=ORIENTED_EDGE('',*,*,#11839,.F.);
#16835=ORIENTED_EDGE('',*,*,#11840,.F.);
#16836=ORIENTED_EDGE('',*,*,#11837,.F.);
#16837=ORIENTED_EDGE('',*,*,#11841,.F.);
#16838=ORIENTED_EDGE('',*,*,#11842,.T.);
#16839=ORIENTED_EDGE('',*,*,#11843,.F.);
#16840=ORIENTED_EDGE('',*,*,#11841,.T.);
#16841=ORIENTED_EDGE('',*,*,#11766,.T.);
#16842=ORIENTED_EDGE('',*,*,#11844,.F.);
#16843=ORIENTED_EDGE('',*,*,#11845,.F.);
#16844=ORIENTED_EDGE('',*,*,#11842,.F.);
#16845=ORIENTED_EDGE('',*,*,#11846,.F.);
#16846=ORIENTED_EDGE('',*,*,#11847,.F.);
#16847=ORIENTED_EDGE('',*,*,#11848,.F.);
#16848=ORIENTED_EDGE('',*,*,#11849,.T.);
#16849=ORIENTED_EDGE('',*,*,#11850,.T.);
#16850=ORIENTED_EDGE('',*,*,#10172,.T.);
#16851=ORIENTED_EDGE('',*,*,#11851,.T.);
#16852=ORIENTED_EDGE('',*,*,#11852,.T.);
#16853=ORIENTED_EDGE('',*,*,#11853,.F.);
#16854=ORIENTED_EDGE('',*,*,#11789,.F.);
#16855=ORIENTED_EDGE('',*,*,#11854,.F.);
#16856=ORIENTED_EDGE('',*,*,#10175,.F.);
#16857=ORIENTED_EDGE('',*,*,#11768,.F.);
#16858=ORIENTED_EDGE('',*,*,#11699,.T.);
#16859=ORIENTED_EDGE('',*,*,#11767,.F.);
#16860=ORIENTED_EDGE('',*,*,#11710,.T.);
#16861=ORIENTED_EDGE('',*,*,#11769,.F.);
#16862=ORIENTED_EDGE('',*,*,#10173,.F.);
#16863=ORIENTED_EDGE('',*,*,#11850,.F.);
#16864=ORIENTED_EDGE('',*,*,#11855,.T.);
#16865=ORIENTED_EDGE('',*,*,#11856,.F.);
#16866=ORIENTED_EDGE('',*,*,#11771,.F.);
#16867=ORIENTED_EDGE('',*,*,#11857,.F.);
#16868=ORIENTED_EDGE('',*,*,#11858,.T.);
#16869=ORIENTED_EDGE('',*,*,#11859,.F.);
#16870=ORIENTED_EDGE('',*,*,#11773,.F.);
#16871=ORIENTED_EDGE('',*,*,#11860,.F.);
#16872=ORIENTED_EDGE('',*,*,#11861,.T.);
#16873=ORIENTED_EDGE('',*,*,#11862,.F.);
#16874=ORIENTED_EDGE('',*,*,#10178,.T.);
#16875=ORIENTED_EDGE('',*,*,#11863,.F.);
#16876=ORIENTED_EDGE('',*,*,#11804,.T.);
#16877=ORIENTED_EDGE('',*,*,#11864,.F.);
#16878=ORIENTED_EDGE('',*,*,#11865,.T.);
#16879=ORIENTED_EDGE('',*,*,#11857,.T.);
#16880=ORIENTED_EDGE('',*,*,#11770,.T.);
#16881=ORIENTED_EDGE('',*,*,#11856,.T.);
#16882=ORIENTED_EDGE('',*,*,#11866,.T.);
#16883=ORIENTED_EDGE('',*,*,#11860,.T.);
#16884=ORIENTED_EDGE('',*,*,#11772,.T.);
#16885=ORIENTED_EDGE('',*,*,#11859,.T.);
#16886=ORIENTED_EDGE('',*,*,#11805,.T.);
#16887=ORIENTED_EDGE('',*,*,#11863,.T.);
#16888=ORIENTED_EDGE('',*,*,#10184,.T.);
#16889=ORIENTED_EDGE('',*,*,#11774,.T.);
#16890=ORIENTED_EDGE('',*,*,#10179,.T.);
#16891=ORIENTED_EDGE('',*,*,#11862,.T.);
#16892=ORIENTED_EDGE('',*,*,#11867,.T.);
#16893=ORIENTED_EDGE('',*,*,#11868,.F.);
#16894=ORIENTED_EDGE('',*,*,#11775,.T.);
#16895=ORIENTED_EDGE('',*,*,#11786,.T.);
#16896=ORIENTED_EDGE('',*,*,#11868,.T.);
#16897=ORIENTED_EDGE('',*,*,#11869,.T.);
#16898=ORIENTED_EDGE('',*,*,#11779,.T.);
#16899=ORIENTED_EDGE('',*,*,#11784,.F.);
#16900=ORIENTED_EDGE('',*,*,#11781,.F.);
#16901=ORIENTED_EDGE('',*,*,#11777,.F.);
#16902=ORIENTED_EDGE('',*,*,#11870,.T.);
#16903=ORIENTED_EDGE('',*,*,#11871,.T.);
#16904=ORIENTED_EDGE('',*,*,#11872,.F.);
#16905=ORIENTED_EDGE('',*,*,#11782,.T.);
#16906=ORIENTED_EDGE('',*,*,#11873,.T.);
#16907=ORIENTED_EDGE('',*,*,#11874,.F.);
#16908=ORIENTED_EDGE('',*,*,#11846,.T.);
#16909=ORIENTED_EDGE('',*,*,#11785,.T.);
#16910=ORIENTED_EDGE('',*,*,#11787,.T.);
#16911=ORIENTED_EDGE('',*,*,#11872,.T.);
#16912=ORIENTED_EDGE('',*,*,#11790,.T.);
#16913=ORIENTED_EDGE('',*,*,#11875,.T.);
#16914=ORIENTED_EDGE('',*,*,#10176,.T.);
#16915=ORIENTED_EDGE('',*,*,#11854,.T.);
#16916=ORIENTED_EDGE('',*,*,#11788,.T.);
#16917=ORIENTED_EDGE('',*,*,#11853,.T.);
#16918=ORIENTED_EDGE('',*,*,#11876,.T.);
#16919=ORIENTED_EDGE('',*,*,#11877,.F.);
#16920=ORIENTED_EDGE('',*,*,#11847,.T.);
#16921=ORIENTED_EDGE('',*,*,#11874,.T.);
#16922=ORIENTED_EDGE('',*,*,#11878,.T.);
#16923=ORIENTED_EDGE('',*,*,#11879,.T.);
#16924=ORIENTED_EDGE('',*,*,#11880,.T.);
#16925=ORIENTED_EDGE('',*,*,#11851,.F.);
#16926=ORIENTED_EDGE('',*,*,#10171,.F.);
#16927=ORIENTED_EDGE('',*,*,#10177,.F.);
#16928=ORIENTED_EDGE('',*,*,#11875,.F.);
#16929=ORIENTED_EDGE('',*,*,#11791,.F.);
#16930=ORIENTED_EDGE('',*,*,#11879,.F.);
#16931=ORIENTED_EDGE('',*,*,#11881,.F.);
#16932=ORIENTED_EDGE('',*,*,#11797,.T.);
#16933=ORIENTED_EDGE('',*,*,#11796,.T.);
#16934=ORIENTED_EDGE('',*,*,#11803,.T.);
#16935=ORIENTED_EDGE('',*,*,#10155,.F.);
#16936=ORIENTED_EDGE('',*,*,#11882,.T.);
#16937=ORIENTED_EDGE('',*,*,#11881,.T.);
#16938=ORIENTED_EDGE('',*,*,#11883,.T.);
#16939=ORIENTED_EDGE('',*,*,#11884,.F.);
#16940=ORIENTED_EDGE('',*,*,#11798,.T.);
#16941=ORIENTED_EDGE('',*,*,#11885,.F.);
#16942=ORIENTED_EDGE('',*,*,#11799,.T.);
#16943=ORIENTED_EDGE('',*,*,#11884,.T.);
#16944=ORIENTED_EDGE('',*,*,#11886,.T.);
#16945=ORIENTED_EDGE('',*,*,#10164,.F.);
#16946=ORIENTED_EDGE('',*,*,#11792,.T.);
#16947=ORIENTED_EDGE('',*,*,#11802,.T.);
#16948=ORIENTED_EDGE('',*,*,#11800,.T.);
#16949=ORIENTED_EDGE('',*,*,#11885,.T.);
#16950=ORIENTED_EDGE('',*,*,#11887,.T.);
#16951=ORIENTED_EDGE('',*,*,#11888,.T.);
#16952=ORIENTED_EDGE('',*,*,#11889,.F.);
#16953=ORIENTED_EDGE('',*,*,#11890,.T.);
#16954=ORIENTED_EDGE('',*,*,#11864,.T.);
#16955=ORIENTED_EDGE('',*,*,#11809,.T.);
#16956=ORIENTED_EDGE('',*,*,#11891,.F.);
#16957=ORIENTED_EDGE('',*,*,#10140,.T.);
#16958=ORIENTED_EDGE('',*,*,#11892,.T.);
#16959=ORIENTED_EDGE('',*,*,#11893,.F.);
#16960=ORIENTED_EDGE('',*,*,#11894,.T.);
#16961=ORIENTED_EDGE('',*,*,#11889,.T.);
#16962=ORIENTED_EDGE('',*,*,#11895,.T.);
#16963=ORIENTED_EDGE('',*,*,#11891,.T.);
#16964=ORIENTED_EDGE('',*,*,#11808,.T.);
#16965=ORIENTED_EDGE('',*,*,#11896,.F.);
#16966=ORIENTED_EDGE('',*,*,#11807,.T.);
#16967=ORIENTED_EDGE('',*,*,#11811,.T.);
#16968=ORIENTED_EDGE('',*,*,#11814,.T.);
#16969=ORIENTED_EDGE('',*,*,#11897,.F.);
#16970=ORIENTED_EDGE('',*,*,#11813,.T.);
#16971=ORIENTED_EDGE('',*,*,#11816,.T.);
#16972=ORIENTED_EDGE('',*,*,#11817,.T.);
#16973=ORIENTED_EDGE('',*,*,#11898,.F.);
#16974=ORIENTED_EDGE('',*,*,#11827,.T.);
#16975=ORIENTED_EDGE('',*,*,#11899,.F.);
#16976=ORIENTED_EDGE('',*,*,#10151,.T.);
#16977=ORIENTED_EDGE('',*,*,#10148,.T.);
#16978=ORIENTED_EDGE('',*,*,#11900,.F.);
#16979=ORIENTED_EDGE('',*,*,#11819,.T.);
#16980=ORIENTED_EDGE('',*,*,#11821,.T.);
#16981=ORIENTED_EDGE('',*,*,#11901,.F.);
#16982=ORIENTED_EDGE('',*,*,#11902,.F.);
#16983=ORIENTED_EDGE('',*,*,#11826,.T.);
#16984=ORIENTED_EDGE('',*,*,#11903,.F.);
#16985=ORIENTED_EDGE('',*,*,#11904,.F.);
#16986=ORIENTED_EDGE('',*,*,#11903,.T.);
#16987=ORIENTED_EDGE('',*,*,#11825,.T.);
#16988=ORIENTED_EDGE('',*,*,#11905,.F.);
#16989=ORIENTED_EDGE('',*,*,#10137,.T.);
#16990=ORIENTED_EDGE('',*,*,#11906,.F.);
#16991=ORIENTED_EDGE('',*,*,#11905,.T.);
#16992=ORIENTED_EDGE('',*,*,#11824,.T.);
#16993=ORIENTED_EDGE('',*,*,#11907,.F.);
#16994=ORIENTED_EDGE('',*,*,#11908,.F.);
#16995=ORIENTED_EDGE('',*,*,#11909,.F.);
#16996=ORIENTED_EDGE('',*,*,#11910,.F.);
#16997=ORIENTED_EDGE('',*,*,#11823,.T.);
#16998=ORIENTED_EDGE('',*,*,#11911,.F.);
#16999=ORIENTED_EDGE('',*,*,#11912,.F.);
#17000=ORIENTED_EDGE('',*,*,#11822,.T.);
#17001=ORIENTED_EDGE('',*,*,#11913,.F.);
#17002=ORIENTED_EDGE('',*,*,#11914,.F.);
#17003=ORIENTED_EDGE('',*,*,#11913,.T.);
#17004=ORIENTED_EDGE('',*,*,#11831,.T.);
#17005=ORIENTED_EDGE('',*,*,#11915,.F.);
#17006=ORIENTED_EDGE('',*,*,#10143,.T.);
#17007=ORIENTED_EDGE('',*,*,#11916,.F.);
#17008=ORIENTED_EDGE('',*,*,#11915,.T.);
#17009=ORIENTED_EDGE('',*,*,#11830,.T.);
#17010=ORIENTED_EDGE('',*,*,#11917,.F.);
#17011=ORIENTED_EDGE('',*,*,#11829,.T.);
#17012=ORIENTED_EDGE('',*,*,#11833,.T.);
#17013=ORIENTED_EDGE('',*,*,#11835,.T.);
#17014=ORIENTED_EDGE('',*,*,#11918,.F.);
#17015=ORIENTED_EDGE('',*,*,#11840,.T.);
#17016=ORIENTED_EDGE('',*,*,#11919,.F.);
#17017=ORIENTED_EDGE('',*,*,#11834,.T.);
#17018=ORIENTED_EDGE('',*,*,#11838,.T.);
#17019=ORIENTED_EDGE('',*,*,#11845,.T.);
#17020=ORIENTED_EDGE('',*,*,#11920,.F.);
#17021=ORIENTED_EDGE('',*,*,#11839,.T.);
#17022=ORIENTED_EDGE('',*,*,#11843,.T.);
#17023=ORIENTED_EDGE('',*,*,#11921,.T.);
#17024=ORIENTED_EDGE('',*,*,#11922,.F.);
#17025=ORIENTED_EDGE('',*,*,#11848,.T.);
#17026=ORIENTED_EDGE('',*,*,#11877,.T.);
#17027=ORIENTED_EDGE('',*,*,#11923,.T.);
#17028=ORIENTED_EDGE('',*,*,#11924,.F.);
#17029=ORIENTED_EDGE('',*,*,#10146,.T.);
#17030=ORIENTED_EDGE('',*,*,#11925,.T.);
#17031=ORIENTED_EDGE('',*,*,#11926,.F.);
#17032=ORIENTED_EDGE('',*,*,#11844,.T.);
#17033=ORIENTED_EDGE('',*,*,#11922,.T.);
#17034=ORIENTED_EDGE('',*,*,#11927,.T.);
#17035=ORIENTED_EDGE('',*,*,#11924,.T.);
#17036=ORIENTED_EDGE('',*,*,#11928,.T.);
#17037=ORIENTED_EDGE('',*,*,#11929,.F.);
#17038=ORIENTED_EDGE('',*,*,#11880,.F.);
#17039=ORIENTED_EDGE('',*,*,#11878,.F.);
#17040=ORIENTED_EDGE('',*,*,#11873,.F.);
#17041=ORIENTED_EDGE('',*,*,#11871,.F.);
#17042=ORIENTED_EDGE('',*,*,#11870,.F.);
#17043=ORIENTED_EDGE('',*,*,#11869,.F.);
#17044=ORIENTED_EDGE('',*,*,#11867,.F.);
#17045=ORIENTED_EDGE('',*,*,#11861,.F.);
#17046=ORIENTED_EDGE('',*,*,#11858,.F.);
#17047=ORIENTED_EDGE('',*,*,#11866,.F.);
#17048=ORIENTED_EDGE('',*,*,#11855,.F.);
#17049=ORIENTED_EDGE('',*,*,#11865,.F.);
#17050=ORIENTED_EDGE('',*,*,#11890,.F.);
#17051=ORIENTED_EDGE('',*,*,#11894,.F.);
#17052=ORIENTED_EDGE('',*,*,#11930,.F.);
#17053=ORIENTED_EDGE('',*,*,#11931,.F.);
#17054=ORIENTED_EDGE('',*,*,#11932,.F.);
#17055=ORIENTED_EDGE('',*,*,#11928,.F.);
#17056=ORIENTED_EDGE('',*,*,#11923,.F.);
#17057=ORIENTED_EDGE('',*,*,#11876,.F.);
#17058=ORIENTED_EDGE('',*,*,#11852,.F.);
#17059=ORIENTED_EDGE('',*,*,#11849,.F.);
#17060=ORIENTED_EDGE('',*,*,#10166,.F.);
#17061=ORIENTED_EDGE('',*,*,#10154,.F.);
#17062=ORIENTED_EDGE('',*,*,#10160,.F.);
#17063=ORIENTED_EDGE('',*,*,#10165,.F.);
#17064=ORIENTED_EDGE('',*,*,#11887,.F.);
#17065=ORIENTED_EDGE('',*,*,#11886,.F.);
#17066=ORIENTED_EDGE('',*,*,#11883,.F.);
#17067=ORIENTED_EDGE('',*,*,#11882,.F.);
#17068=ORIENTED_EDGE('',*,*,#11933,.T.);
#17069=ORIENTED_EDGE('',*,*,#11934,.F.);
#17070=ORIENTED_EDGE('',*,*,#11930,.T.);
#17071=ORIENTED_EDGE('',*,*,#11893,.T.);
#17072=ORIENTED_EDGE('',*,*,#11933,.F.);
#17073=ORIENTED_EDGE('',*,*,#11892,.F.);
#17074=ORIENTED_EDGE('',*,*,#11888,.F.);
#17075=ORIENTED_EDGE('',*,*,#11895,.F.);
#17076=ORIENTED_EDGE('',*,*,#11935,.F.);
#17077=ORIENTED_EDGE('',*,*,#11936,.F.);
#17078=ORIENTED_EDGE('',*,*,#11898,.T.);
#17079=ORIENTED_EDGE('',*,*,#11900,.T.);
#17080=ORIENTED_EDGE('',*,*,#10147,.T.);
#17081=ORIENTED_EDGE('',*,*,#11899,.T.);
#17082=ORIENTED_EDGE('',*,*,#11902,.T.);
#17083=ORIENTED_EDGE('',*,*,#11937,.F.);
#17084=ORIENTED_EDGE('',*,*,#11938,.F.);
#17085=ORIENTED_EDGE('',*,*,#11935,.T.);
#17086=ORIENTED_EDGE('',*,*,#11896,.T.);
#17087=ORIENTED_EDGE('',*,*,#11897,.T.);
#17088=ORIENTED_EDGE('',*,*,#11904,.T.);
#17089=ORIENTED_EDGE('',*,*,#11906,.T.);
#17090=ORIENTED_EDGE('',*,*,#11939,.F.);
#17091=ORIENTED_EDGE('',*,*,#11940,.F.);
#17092=ORIENTED_EDGE('',*,*,#11937,.T.);
#17093=ORIENTED_EDGE('',*,*,#11901,.T.);
#17094=ORIENTED_EDGE('',*,*,#11907,.T.);
#17095=ORIENTED_EDGE('',*,*,#11910,.T.);
#17096=ORIENTED_EDGE('',*,*,#11941,.F.);
#17097=ORIENTED_EDGE('',*,*,#11942,.F.);
#17098=ORIENTED_EDGE('',*,*,#11939,.T.);
#17099=ORIENTED_EDGE('',*,*,#11943,.F.);
#17100=ORIENTED_EDGE('',*,*,#11944,.F.);
#17101=ORIENTED_EDGE('',*,*,#11941,.T.);
#17102=ORIENTED_EDGE('',*,*,#11909,.T.);
#17103=ORIENTED_EDGE('',*,*,#11945,.F.);
#17104=ORIENTED_EDGE('',*,*,#11946,.F.);
#17105=ORIENTED_EDGE('',*,*,#11943,.T.);
#17106=ORIENTED_EDGE('',*,*,#11908,.T.);
#17107=ORIENTED_EDGE('',*,*,#11912,.T.);
#17108=ORIENTED_EDGE('',*,*,#11914,.T.);
#17109=ORIENTED_EDGE('',*,*,#11916,.T.);
#17110=ORIENTED_EDGE('',*,*,#11947,.F.);
#17111=ORIENTED_EDGE('',*,*,#11948,.F.);
#17112=ORIENTED_EDGE('',*,*,#11945,.T.);
#17113=ORIENTED_EDGE('',*,*,#11911,.T.);
#17114=ORIENTED_EDGE('',*,*,#11949,.T.);
#17115=ORIENTED_EDGE('',*,*,#11950,.F.);
#17116=ORIENTED_EDGE('',*,*,#11947,.T.);
#17117=ORIENTED_EDGE('',*,*,#11917,.T.);
#17118=ORIENTED_EDGE('',*,*,#11918,.T.);
#17119=ORIENTED_EDGE('',*,*,#11919,.T.);
#17120=ORIENTED_EDGE('',*,*,#11920,.T.);
#17121=ORIENTED_EDGE('',*,*,#11926,.T.);
#17122=ORIENTED_EDGE('',*,*,#11949,.F.);
#17123=ORIENTED_EDGE('',*,*,#11925,.F.);
#17124=ORIENTED_EDGE('',*,*,#11921,.F.);
#17125=ORIENTED_EDGE('',*,*,#11927,.F.);
#17126=ORIENTED_EDGE('',*,*,#11951,.F.);
#17127=ORIENTED_EDGE('',*,*,#11952,.F.);
#17128=ORIENTED_EDGE('',*,*,#11951,.T.);
#17129=ORIENTED_EDGE('',*,*,#11929,.T.);
#17130=ORIENTED_EDGE('',*,*,#11932,.T.);
#17131=ORIENTED_EDGE('',*,*,#11953,.F.);
#17132=ORIENTED_EDGE('',*,*,#11952,.T.);
#17133=ORIENTED_EDGE('',*,*,#11953,.T.);
#17134=ORIENTED_EDGE('',*,*,#11931,.T.);
#17135=ORIENTED_EDGE('',*,*,#11934,.T.);
#17136=ORIENTED_EDGE('',*,*,#11936,.T.);
#17137=ORIENTED_EDGE('',*,*,#11938,.T.);
#17138=ORIENTED_EDGE('',*,*,#11940,.T.);
#17139=ORIENTED_EDGE('',*,*,#11942,.T.);
#17140=ORIENTED_EDGE('',*,*,#11944,.T.);
#17141=ORIENTED_EDGE('',*,*,#11946,.T.);
#17142=ORIENTED_EDGE('',*,*,#11948,.T.);
#17143=ORIENTED_EDGE('',*,*,#11950,.T.);
#17144=ORIENTED_EDGE('',*,*,#10135,.T.);
#17145=ORIENTED_EDGE('',*,*,#10138,.T.);
#17146=ORIENTED_EDGE('',*,*,#10141,.T.);
#17147=ORIENTED_EDGE('',*,*,#10144,.T.);
#17148=ORIENTED_EDGE('',*,*,#11954,.F.);
#17149=ORIENTED_EDGE('',*,*,#11955,.F.);
#17150=ORIENTED_EDGE('',*,*,#11956,.T.);
#17151=ORIENTED_EDGE('',*,*,#11957,.F.);
#17152=ORIENTED_EDGE('',*,*,#11956,.F.);
#17153=ORIENTED_EDGE('',*,*,#11958,.F.);
#17154=ORIENTED_EDGE('',*,*,#11959,.F.);
#17155=ORIENTED_EDGE('',*,*,#11960,.F.);
#17156=ORIENTED_EDGE('',*,*,#11961,.T.);
#17157=ORIENTED_EDGE('',*,*,#11962,.F.);
#17158=ORIENTED_EDGE('',*,*,#11961,.F.);
#17159=ORIENTED_EDGE('',*,*,#11963,.F.);
#17160=ORIENTED_EDGE('',*,*,#11964,.F.);
#17161=ORIENTED_EDGE('',*,*,#11965,.F.);
#17162=ORIENTED_EDGE('',*,*,#11966,.F.);
#17163=ORIENTED_EDGE('',*,*,#11967,.T.);
#17164=ORIENTED_EDGE('',*,*,#11968,.T.);
#17165=ORIENTED_EDGE('',*,*,#11967,.F.);
#17166=ORIENTED_EDGE('',*,*,#11954,.T.);
#17167=ORIENTED_EDGE('',*,*,#11955,.T.);
#17168=ORIENTED_EDGE('',*,*,#11969,.T.);
#17169=ORIENTED_EDGE('',*,*,#11966,.T.);
#17170=ORIENTED_EDGE('',*,*,#11969,.F.);
#17171=ORIENTED_EDGE('',*,*,#11962,.T.);
#17172=ORIENTED_EDGE('',*,*,#11957,.T.);
#17173=ORIENTED_EDGE('',*,*,#11968,.F.);
#17174=ORIENTED_EDGE('',*,*,#11970,.T.);
#17175=ORIENTED_EDGE('',*,*,#11963,.T.);
#17176=ORIENTED_EDGE('',*,*,#11971,.T.);
#17177=ORIENTED_EDGE('',*,*,#11972,.T.);
#17178=ORIENTED_EDGE('',*,*,#11973,.T.);
#17179=ORIENTED_EDGE('',*,*,#11964,.T.);
#17180=ORIENTED_EDGE('',*,*,#11974,.T.);
#17181=ORIENTED_EDGE('',*,*,#11975,.T.);
#17182=ORIENTED_EDGE('',*,*,#11965,.T.);
#17183=ORIENTED_EDGE('',*,*,#11976,.T.);
#17184=ORIENTED_EDGE('',*,*,#11977,.T.);
#17185=ORIENTED_EDGE('',*,*,#11958,.T.);
#17186=ORIENTED_EDGE('',*,*,#11978,.T.);
#17187=ORIENTED_EDGE('',*,*,#11979,.T.);
#17188=ORIENTED_EDGE('',*,*,#11959,.T.);
#17189=ORIENTED_EDGE('',*,*,#11980,.T.);
#17190=ORIENTED_EDGE('',*,*,#11981,.T.);
#17191=ORIENTED_EDGE('',*,*,#11960,.T.);
#17192=ORIENTED_EDGE('',*,*,#11982,.F.);
#17193=ORIENTED_EDGE('',*,*,#11983,.F.);
#17194=ORIENTED_EDGE('',*,*,#11984,.F.);
#17195=ORIENTED_EDGE('',*,*,#11985,.F.);
#17196=ORIENTED_EDGE('',*,*,#11986,.T.);
#17197=ORIENTED_EDGE('',*,*,#11987,.F.);
#17198=ORIENTED_EDGE('',*,*,#11988,.T.);
#17199=ORIENTED_EDGE('',*,*,#11989,.T.);
#17200=ORIENTED_EDGE('',*,*,#11987,.T.);
#17201=ORIENTED_EDGE('',*,*,#11990,.T.);
#17202=ORIENTED_EDGE('',*,*,#11991,.T.);
#17203=ORIENTED_EDGE('',*,*,#11986,.F.);
#17204=ORIENTED_EDGE('',*,*,#11992,.T.);
#17205=ORIENTED_EDGE('',*,*,#11985,.T.);
#17206=ORIENTED_EDGE('',*,*,#11993,.T.);
#17207=ORIENTED_EDGE('',*,*,#11994,.T.);
#17208=ORIENTED_EDGE('',*,*,#11984,.T.);
#17209=ORIENTED_EDGE('',*,*,#11995,.T.);
#17210=ORIENTED_EDGE('',*,*,#11996,.T.);
#17211=ORIENTED_EDGE('',*,*,#11997,.T.);
#17212=ORIENTED_EDGE('',*,*,#11982,.T.);
#17213=ORIENTED_EDGE('',*,*,#11998,.T.);
#17214=ORIENTED_EDGE('',*,*,#11983,.T.);
#17215=ORIENTED_EDGE('',*,*,#11999,.T.);
#17216=ORIENTED_EDGE('',*,*,#11981,.F.);
#17217=ORIENTED_EDGE('',*,*,#12000,.T.);
#17218=ORIENTED_EDGE('',*,*,#11999,.F.);
#17219=ORIENTED_EDGE('',*,*,#11997,.F.);
#17220=ORIENTED_EDGE('',*,*,#12001,.F.);
#17221=ORIENTED_EDGE('',*,*,#11971,.F.);
#17222=ORIENTED_EDGE('',*,*,#11979,.F.);
#17223=ORIENTED_EDGE('',*,*,#12002,.T.);
#17224=ORIENTED_EDGE('',*,*,#11995,.F.);
#17225=ORIENTED_EDGE('',*,*,#11998,.F.);
#17226=ORIENTED_EDGE('',*,*,#12000,.F.);
#17227=ORIENTED_EDGE('',*,*,#11980,.F.);
#17228=ORIENTED_EDGE('',*,*,#11977,.F.);
#17229=ORIENTED_EDGE('',*,*,#12003,.T.);
#17230=ORIENTED_EDGE('',*,*,#11993,.F.);
#17231=ORIENTED_EDGE('',*,*,#11994,.F.);
#17232=ORIENTED_EDGE('',*,*,#12002,.F.);
#17233=ORIENTED_EDGE('',*,*,#11978,.F.);
#17234=ORIENTED_EDGE('',*,*,#11975,.F.);
#17235=ORIENTED_EDGE('',*,*,#12004,.T.);
#17236=ORIENTED_EDGE('',*,*,#11990,.F.);
#17237=ORIENTED_EDGE('',*,*,#11992,.F.);
#17238=ORIENTED_EDGE('',*,*,#12003,.F.);
#17239=ORIENTED_EDGE('',*,*,#11976,.F.);
#17240=ORIENTED_EDGE('',*,*,#11973,.F.);
#17241=ORIENTED_EDGE('',*,*,#12005,.T.);
#17242=ORIENTED_EDGE('',*,*,#11988,.F.);
#17243=ORIENTED_EDGE('',*,*,#11991,.F.);
#17244=ORIENTED_EDGE('',*,*,#12004,.F.);
#17245=ORIENTED_EDGE('',*,*,#11974,.F.);
#17246=ORIENTED_EDGE('',*,*,#11970,.F.);
#17247=ORIENTED_EDGE('',*,*,#12001,.T.);
#17248=ORIENTED_EDGE('',*,*,#11996,.F.);
#17249=ORIENTED_EDGE('',*,*,#11989,.F.);
#17250=ORIENTED_EDGE('',*,*,#12005,.F.);
#17251=ORIENTED_EDGE('',*,*,#11972,.F.);
#17252=TOROIDAL_SURFACE('',#18351,30.,5.);
#17253=TOROIDAL_SURFACE('',#18355,245.,5.);
#17254=TOROIDAL_SURFACE('',#18722,222.,14.);
#17255=TOROIDAL_SURFACE('',#18729,222.,15.);
#17256=TOROIDAL_SURFACE('',#18853,29.0000000000007,5.00000000000101);
#17257=TOROIDAL_SURFACE('',#18858,27.0000000000009,4.99999999999874);
#17258=TOROIDAL_SURFACE('',#18864,45.5,4.00000000000009);
#17259=TOROIDAL_SURFACE('',#18870,35.0000000000004,3.99999999999933);
#17260=TOROIDAL_SURFACE('',#18905,25.3774921629995,19.9999999999997);
#17261=TOROIDAL_SURFACE('',#19945,2.2,0.2);
#17262=ADVANCED_FACE('',(#4822),#17252,.T.);
#17263=ADVANCED_FACE('',(#4823),#17253,.T.);
#17264=ADVANCED_FACE('',(#4824),#4554,.T.);
#17265=ADVANCED_FACE('',(#4825),#4555,.F.);
#17266=ADVANCED_FACE('',(#4826),#4556,.F.);
#17267=ADVANCED_FACE('',(#4827),#4557,.F.);
#17268=ADVANCED_FACE('',(#4828),#4558,.F.);
#17269=ADVANCED_FACE('',(#4829),#4559,.F.);
#17270=ADVANCED_FACE('',(#4830),#4560,.F.);
#17271=ADVANCED_FACE('',(#4831),#4561,.F.);
#17272=ADVANCED_FACE('',(#4832),#4562,.F.);
#17273=ADVANCED_FACE('',(#4833),#4563,.T.);
#17274=ADVANCED_FACE('',(#4834),#4564,.T.);
#17275=ADVANCED_FACE('',(#4835),#4565,.F.);
#17276=ADVANCED_FACE('',(#4836),#4566,.F.);
#17277=ADVANCED_FACE('',(#4837),#4567,.F.);
#17278=ADVANCED_FACE('',(#4838),#4568,.F.);
#17279=ADVANCED_FACE('',(#4839),#4569,.F.);
#17280=ADVANCED_FACE('',(#4840),#4570,.F.);
#17281=ADVANCED_FACE('',(#4841),#4571,.F.);
#17282=ADVANCED_FACE('',(#4842),#4572,.F.);
#17283=ADVANCED_FACE('',(#4843),#4573,.F.);
#17284=ADVANCED_FACE('',(#4844),#4574,.F.);
#17285=ADVANCED_FACE('',(#4845),#4575,.F.);
#17286=ADVANCED_FACE('',(#4846),#4576,.F.);
#17287=ADVANCED_FACE('',(#4847),#4577,.F.);
#17288=ADVANCED_FACE('',(#4848),#4578,.F.);
#17289=ADVANCED_FACE('',(#4849),#4579,.F.);
#17290=ADVANCED_FACE('',(#4850),#4580,.F.);
#17291=ADVANCED_FACE('',(#4851),#4581,.F.);
#17292=ADVANCED_FACE('',(#4852),#4582,.F.);
#17293=ADVANCED_FACE('',(#4853,#876,#877),#4583,.T.);
#17294=ADVANCED_FACE('',(#4854),#4584,.T.);
#17295=ADVANCED_FACE('',(#4855,#878,#879),#4585,.F.);
#17296=ADVANCED_FACE('',(#4856,#880),#297,.T.);
#17297=ADVANCED_FACE('',(#4857,#881,#882,#883,#884,#885,#886,#887,#888,
#889,#890,#891,#892,#893,#894,#895,#896),#298,.T.);
#17298=ADVANCED_FACE('',(#4858,#897,#898,#899,#900,#901,#902,#903,#904,
#905,#906,#907,#908,#909,#910,#911,#912),#299,.F.);
#17299=ADVANCED_FACE('',(#4859,#913),#300,.F.);
#17300=ADVANCED_FACE('',(#4860,#914,#915,#916,#917,#918),#301,.T.);
#17301=ADVANCED_FACE('',(#4861,#919,#920,#921,#922,#923),#302,.F.);
#17302=ADVANCED_FACE('',(#4862),#4586,.T.);
#17303=ADVANCED_FACE('',(#4863),#303,.F.);
#17304=ADVANCED_FACE('',(#4864),#4587,.T.);
#17305=ADVANCED_FACE('',(#4865),#304,.F.);
#17306=ADVANCED_FACE('',(#4866),#4588,.T.);
#17307=ADVANCED_FACE('',(#4867),#305,.F.);
#17308=ADVANCED_FACE('',(#4868),#4589,.T.);
#17309=ADVANCED_FACE('',(#4869),#306,.F.);
#17310=ADVANCED_FACE('',(#4870,#924,#925,#926,#927,#928),#307,.T.);
#17311=ADVANCED_FACE('',(#4871,#929,#930,#931,#932,#933),#308,.F.);
#17312=ADVANCED_FACE('',(#4872),#4590,.T.);
#17313=ADVANCED_FACE('',(#4873),#309,.F.);
#17314=ADVANCED_FACE('',(#4874),#4591,.T.);
#17315=ADVANCED_FACE('',(#4875),#310,.F.);
#17316=ADVANCED_FACE('',(#4876),#4592,.T.);
#17317=ADVANCED_FACE('',(#4877),#311,.F.);
#17318=ADVANCED_FACE('',(#4878),#4593,.T.);
#17319=ADVANCED_FACE('',(#4879),#312,.F.);
#17320=ADVANCED_FACE('',(#4880,#934),#313,.T.);
#17321=ADVANCED_FACE('',(#4881),#314,.T.);
#17322=ADVANCED_FACE('',(#4882),#315,.F.);
#17323=ADVANCED_FACE('',(#4883),#316,.F.);
#17324=ADVANCED_FACE('',(#4884),#317,.T.);
#17325=ADVANCED_FACE('',(#4885),#318,.F.);
#17326=ADVANCED_FACE('',(#4886),#319,.F.);
#17327=ADVANCED_FACE('',(#4887),#320,.T.);
#17328=ADVANCED_FACE('',(#4888),#321,.F.);
#17329=ADVANCED_FACE('',(#4889),#322,.F.);
#17330=ADVANCED_FACE('',(#4890),#323,.T.);
#17331=ADVANCED_FACE('',(#4891),#324,.F.);
#17332=ADVANCED_FACE('',(#4892),#325,.F.);
#17333=ADVANCED_FACE('',(#4893),#326,.T.);
#17334=ADVANCED_FACE('',(#4894),#327,.F.);
#17335=ADVANCED_FACE('',(#4895),#328,.F.);
#17336=ADVANCED_FACE('',(#4896),#329,.T.);
#17337=ADVANCED_FACE('',(#4897),#330,.F.);
#17338=ADVANCED_FACE('',(#4898),#331,.F.);
#17339=ADVANCED_FACE('',(#4899),#332,.T.);
#17340=ADVANCED_FACE('',(#4900),#333,.F.);
#17341=ADVANCED_FACE('',(#4901),#334,.F.);
#17342=ADVANCED_FACE('',(#4902),#335,.T.);
#17343=ADVANCED_FACE('',(#4903),#336,.F.);
#17344=ADVANCED_FACE('',(#4904),#337,.F.);
#17345=ADVANCED_FACE('',(#4905),#338,.T.);
#17346=ADVANCED_FACE('',(#4906),#339,.F.);
#17347=ADVANCED_FACE('',(#4907),#340,.F.);
#17348=ADVANCED_FACE('',(#4908),#4594,.T.);
#17349=ADVANCED_FACE('',(#4909),#4595,.F.);
#17350=ADVANCED_FACE('',(#4910),#4596,.F.);
#17351=ADVANCED_FACE('',(#4911),#4597,.T.);
#17352=ADVANCED_FACE('',(#4912,#935),#341,.F.);
#17353=ADVANCED_FACE('',(#4913,#936),#342,.T.);
#17354=ADVANCED_FACE('',(#4914),#343,.T.);
#17355=ADVANCED_FACE('',(#4915),#4598,.F.);
#17356=ADVANCED_FACE('',(#4916),#4599,.T.);
#17357=ADVANCED_FACE('',(#4917),#344,.T.);
#17358=ADVANCED_FACE('',(#4918),#345,.T.);
#17359=ADVANCED_FACE('',(#4919),#4600,.T.);
#17360=ADVANCED_FACE('',(#4920),#4601,.T.);
#17361=ADVANCED_FACE('',(#4921),#4602,.T.);
#17362=ADVANCED_FACE('',(#4922),#4603,.T.);
#17363=ADVANCED_FACE('',(#4923),#4604,.T.);
#17364=ADVANCED_FACE('',(#4924),#4605,.T.);
#17365=ADVANCED_FACE('',(#4925),#4606,.T.);
#17366=ADVANCED_FACE('',(#4926),#4607,.T.);
#17367=ADVANCED_FACE('',(#4927),#4608,.T.);
#17368=ADVANCED_FACE('',(#4928),#4609,.F.);
#17369=ADVANCED_FACE('',(#4929),#4610,.F.);
#17370=ADVANCED_FACE('',(#4930),#4611,.T.);
#17371=ADVANCED_FACE('',(#4931,#937),#346,.F.);
#17372=ADVANCED_FACE('',(#4932,#938),#347,.T.);
#17373=ADVANCED_FACE('',(#4933),#348,.T.);
#17374=ADVANCED_FACE('',(#4934),#4612,.F.);
#17375=ADVANCED_FACE('',(#4935),#4613,.T.);
#17376=ADVANCED_FACE('',(#4936),#349,.T.);
#17377=ADVANCED_FACE('',(#4937),#350,.T.);
#17378=ADVANCED_FACE('',(#939),#4614,.T.);
#17379=ADVANCED_FACE('',(#940),#4615,.T.);
#17380=ADVANCED_FACE('',(#4938),#4616,.T.);
#17381=ADVANCED_FACE('',(#941),#4617,.T.);
#17382=ADVANCED_FACE('',(#942),#4618,.T.);
#17383=ADVANCED_FACE('',(#4939),#4619,.T.);
#17384=ADVANCED_FACE('',(#4940),#4620,.T.);
#17385=ADVANCED_FACE('',(#4941),#4621,.T.);
#17386=ADVANCED_FACE('',(#4942),#244,.F.);
#17387=ADVANCED_FACE('',(#4943),#4622,.F.);
#17388=ADVANCED_FACE('',(#4944),#4623,.F.);
#17389=ADVANCED_FACE('',(#4945),#245,.T.);
#17390=ADVANCED_FACE('',(#4946),#4624,.F.);
#17391=ADVANCED_FACE('',(#4947),#4625,.F.);
#17392=ADVANCED_FACE('',(#4948),#4626,.T.);
#17393=ADVANCED_FACE('',(#4949,#943),#4627,.T.);
#17394=ADVANCED_FACE('',(#4950,#944,#945,#946,#947,#948),#4628,.F.);
#17395=ADVANCED_FACE('',(#4951,#949),#351,.T.);
#17396=ADVANCED_FACE('',(#4952),#4629,.T.);
#17397=ADVANCED_FACE('',(#4953),#4630,.T.);
#17398=ADVANCED_FACE('',(#4954),#4631,.T.);
#17399=ADVANCED_FACE('',(#4955),#4632,.T.);
#17400=ADVANCED_FACE('',(#4956),#4633,.T.);
#17401=ADVANCED_FACE('',(#4957),#4634,.T.);
#17402=ADVANCED_FACE('',(#4958),#4635,.T.);
#17403=ADVANCED_FACE('',(#4959),#4636,.T.);
#17404=ADVANCED_FACE('',(#4960,#950),#352,.T.);
#17405=ADVANCED_FACE('',(#4961,#951),#353,.F.);
#17406=ADVANCED_FACE('',(#4962),#4637,.F.);
#17407=ADVANCED_FACE('',(#4963),#4638,.T.);
#17408=ADVANCED_FACE('',(#4964),#4639,.F.);
#17409=ADVANCED_FACE('',(#4965),#4640,.F.);
#17410=ADVANCED_FACE('',(#4966),#4641,.T.);
#17411=ADVANCED_FACE('',(#4967),#4642,.F.);
#17412=ADVANCED_FACE('',(#4968,#952),#354,.F.);
#17413=ADVANCED_FACE('',(#4969,#953),#355,.T.);
#17414=ADVANCED_FACE('',(#4970),#4643,.F.);
#17415=ADVANCED_FACE('',(#4971),#356,.F.);
#17416=ADVANCED_FACE('',(#4972),#357,.F.);
#17417=ADVANCED_FACE('',(#4973),#358,.T.);
#17418=ADVANCED_FACE('',(#4974),#359,.F.);
#17419=ADVANCED_FACE('',(#4975),#360,.F.);
#17420=ADVANCED_FACE('',(#4976),#361,.T.);
#17421=ADVANCED_FACE('',(#4977),#362,.F.);
#17422=ADVANCED_FACE('',(#4978),#363,.F.);
#17423=ADVANCED_FACE('',(#4979),#364,.F.);
#17424=ADVANCED_FACE('',(#4980),#365,.F.);
#17425=ADVANCED_FACE('',(#4981),#366,.T.);
#17426=ADVANCED_FACE('',(#4982),#367,.F.);
#17427=ADVANCED_FACE('',(#4983),#368,.F.);
#17428=ADVANCED_FACE('',(#4984),#369,.F.);
#17429=ADVANCED_FACE('',(#4985),#370,.T.);
#17430=ADVANCED_FACE('',(#4986),#371,.F.);
#17431=ADVANCED_FACE('',(#4987),#372,.F.);
#17432=ADVANCED_FACE('',(#4988),#373,.T.);
#17433=ADVANCED_FACE('',(#4989),#374,.F.);
#17434=ADVANCED_FACE('',(#4990),#375,.F.);
#17435=ADVANCED_FACE('',(#4991),#376,.T.);
#17436=ADVANCED_FACE('',(#4992),#377,.F.);
#17437=ADVANCED_FACE('',(#4993),#378,.F.);
#17438=ADVANCED_FACE('',(#4994),#379,.T.);
#17439=ADVANCED_FACE('',(#4995),#380,.F.);
#17440=ADVANCED_FACE('',(#4996),#381,.F.);
#17441=ADVANCED_FACE('',(#4997),#382,.T.);
#17442=ADVANCED_FACE('',(#4998),#383,.F.);
#17443=ADVANCED_FACE('',(#4999),#384,.F.);
#17444=ADVANCED_FACE('',(#5000),#385,.T.);
#17445=ADVANCED_FACE('',(#5001),#246,.T.);
#17446=ADVANCED_FACE('',(#5002),#4644,.F.);
#17447=ADVANCED_FACE('',(#5003),#4645,.F.);
#17448=ADVANCED_FACE('',(#5004),#247,.F.);
#17449=ADVANCED_FACE('',(#5005),#386,.F.);
#17450=ADVANCED_FACE('',(#5006),#387,.F.);
#17451=ADVANCED_FACE('',(#5007),#388,.F.);
#17452=ADVANCED_FACE('',(#5008),#17254,.F.);
#17453=ADVANCED_FACE('',(#5009),#17255,.T.);
#17454=ADVANCED_FACE('',(#5010),#184,.F.);
#17455=ADVANCED_FACE('',(#5011),#4646,.F.);
#17456=ADVANCED_FACE('',(#5012),#4647,.F.);
#17457=ADVANCED_FACE('',(#5013),#185,.T.);
#17458=ADVANCED_FACE('',(#5014),#4648,.T.);
#17459=ADVANCED_FACE('',(#5015),#4649,.T.);
#17460=ADVANCED_FACE('',(#5016,#954),#389,.T.);
#17461=ADVANCED_FACE('',(#5017,#955),#390,.F.);
#17462=ADVANCED_FACE('',(#5018),#4650,.F.);
#17463=ADVANCED_FACE('',(#5019),#186,.T.);
#17464=ADVANCED_FACE('',(#5020),#4651,.T.);
#17465=ADVANCED_FACE('',(#5021),#187,.F.);
#17466=ADVANCED_FACE('',(#5022),#4652,.F.);
#17467=ADVANCED_FACE('',(#5023),#4653,.F.);
#17468=ADVANCED_FACE('',(#5024),#4654,.F.);
#17469=ADVANCED_FACE('',(#5025),#4655,.F.);
#17470=ADVANCED_FACE('',(#5026),#391,.T.);
#17471=ADVANCED_FACE('',(#5027),#392,.T.);
#17472=ADVANCED_FACE('',(#5028),#393,.T.);
#17473=ADVANCED_FACE('',(#5029),#394,.T.);
#17474=ADVANCED_FACE('',(#5030),#395,.T.);
#17475=ADVANCED_FACE('',(#5031),#396,.T.);
#17476=ADVANCED_FACE('',(#5032),#397,.T.);
#17477=ADVANCED_FACE('',(#5033),#398,.T.);
#17478=ADVANCED_FACE('',(#5034),#399,.T.);
#17479=ADVANCED_FACE('',(#5035),#400,.T.);
#17480=ADVANCED_FACE('',(#5036),#401,.T.);
#17481=ADVANCED_FACE('',(#5037),#402,.T.);
#17482=ADVANCED_FACE('',(#5038,#956,#957,#958,#959),#403,.F.);
#17483=ADVANCED_FACE('',(#5039,#960,#961,#962,#963),#404,.T.);
#17484=ADVANCED_FACE('',(#5040),#405,.F.);
#17485=ADVANCED_FACE('',(#5041),#406,.F.);
#17486=ADVANCED_FACE('',(#5042),#407,.F.);
#17487=ADVANCED_FACE('',(#5043),#408,.F.);
#17488=ADVANCED_FACE('',(#5044),#409,.F.);
#17489=ADVANCED_FACE('',(#5045),#410,.F.);
#17490=ADVANCED_FACE('',(#5046),#411,.F.);
#17491=ADVANCED_FACE('',(#5047),#412,.T.);
#17492=ADVANCED_FACE('',(#5048),#413,.T.);
#17493=ADVANCED_FACE('',(#5049),#414,.T.);
#17494=ADVANCED_FACE('',(#5050),#415,.T.);
#17495=ADVANCED_FACE('',(#5051),#416,.F.);
#17496=ADVANCED_FACE('',(#5052),#417,.F.);
#17497=ADVANCED_FACE('',(#5053),#418,.F.);
#17498=ADVANCED_FACE('',(#5054),#4656,.F.);
#17499=ADVANCED_FACE('',(#5055),#4657,.F.);
#17500=ADVANCED_FACE('',(#5056),#4658,.F.);
#17501=ADVANCED_FACE('',(#5057),#4659,.F.);
#17502=ADVANCED_FACE('',(#5058),#4660,.F.);
#17503=ADVANCED_FACE('',(#5059),#4661,.F.);
#17504=ADVANCED_FACE('',(#5060),#4662,.F.);
#17505=ADVANCED_FACE('',(#5061),#4663,.F.);
#17506=ADVANCED_FACE('',(#5062),#4664,.F.);
#17507=ADVANCED_FACE('',(#5063),#4665,.F.);
#17508=ADVANCED_FACE('',(#5064),#4666,.F.);
#17509=ADVANCED_FACE('',(#5065),#4667,.F.);
#17510=ADVANCED_FACE('',(#5066),#4668,.F.);
#17511=ADVANCED_FACE('',(#5067),#4669,.F.);
#17512=ADVANCED_FACE('',(#5068),#4670,.F.);
#17513=ADVANCED_FACE('',(#5069),#4671,.F.);
#17514=ADVANCED_FACE('',(#5070),#4672,.T.);
#17515=ADVANCED_FACE('',(#5071,#964,#965,#966,#967,#968,#969,#970,#971,
#972,#973,#974,#975,#976,#977,#978,#979),#419,.T.);
#17516=ADVANCED_FACE('',(#5072,#980,#981,#982,#983,#984,#985,#986,#987,
#988,#989,#990,#991,#992,#993,#994,#995),#420,.F.);
#17517=ADVANCED_FACE('',(#5073),#4673,.T.);
#17518=ADVANCED_FACE('',(#5074),#421,.F.);
#17519=ADVANCED_FACE('',(#5075),#422,.T.);
#17520=ADVANCED_FACE('',(#5076),#17256,.F.);
#17521=ADVANCED_FACE('',(#5077),#17257,.T.);
#17522=ADVANCED_FACE('',(#5078),#17258,.F.);
#17523=ADVANCED_FACE('',(#5079),#17259,.F.);
#17524=ADVANCED_FACE('',(#5080),#4674,.F.);
#17525=ADVANCED_FACE('',(#5081),#129,.T.);
#17526=ADVANCED_FACE('',(#5082),#130,.F.);
#17527=ADVANCED_FACE('',(#5083),#131,.T.);
#17528=ADVANCED_FACE('',(#5084),#132,.T.);
#17529=ADVANCED_FACE('',(#5085,#996),#423,.F.);
#17530=ADVANCED_FACE('',(#5086,#997),#424,.F.);
#17531=ADVANCED_FACE('',(#5087),#133,.T.);
#17532=ADVANCED_FACE('',(#5088),#134,.F.);
#17533=ADVANCED_FACE('',(#5089,#998),#425,.F.);
#17534=ADVANCED_FACE('',(#5090),#135,.F.);
#17535=ADVANCED_FACE('',(#5091),#426,.T.);
#17536=ADVANCED_FACE('',(#5092),#427,.T.);
#17537=ADVANCED_FACE('',(#5093),#428,.F.);
#17538=ADVANCED_FACE('',(#5094),#429,.F.);
#17539=ADVANCED_FACE('',(#5095),#430,.F.);
#17540=ADVANCED_FACE('',(#5096),#431,.F.);
#17541=ADVANCED_FACE('',(#5097),#432,.F.);
#17542=ADVANCED_FACE('',(#5098),#433,.F.);
#17543=ADVANCED_FACE('',(#5099),#434,.T.);
#17544=ADVANCED_FACE('',(#5100),#435,.T.);
#17545=ADVANCED_FACE('',(#5101),#188,.T.);
#17546=ADVANCED_FACE('',(#5102),#189,.T.);
#17547=ADVANCED_FACE('',(#5103),#17260,.T.);
#17548=ADVANCED_FACE('',(#5104),#4675,.F.);
#17549=ADVANCED_FACE('',(#5105),#4676,.F.);
#17550=ADVANCED_FACE('',(#5106),#4677,.F.);
#17551=ADVANCED_FACE('',(#5107),#4678,.F.);
#17552=ADVANCED_FACE('',(#5108),#4679,.T.);
#17553=ADVANCED_FACE('',(#5109),#4680,.T.);
#17554=ADVANCED_FACE('',(#5110),#136,.T.);
#17555=ADVANCED_FACE('',(#5111),#4681,.T.);
#17556=ADVANCED_FACE('',(#5112),#4682,.T.);
#17557=ADVANCED_FACE('',(#5113),#4683,.T.);
#17558=ADVANCED_FACE('',(#5114),#4684,.T.);
#17559=ADVANCED_FACE('',(#5115),#4685,.T.);
#17560=ADVANCED_FACE('',(#5116),#4686,.T.);
#17561=ADVANCED_FACE('',(#5117),#4687,.F.);
#17562=ADVANCED_FACE('',(#5118),#4688,.F.);
#17563=ADVANCED_FACE('',(#5119),#4689,.F.);
#17564=ADVANCED_FACE('',(#5120),#4690,.F.);
#17565=ADVANCED_FACE('',(#5121),#4691,.F.);
#17566=ADVANCED_FACE('',(#5122),#4692,.T.);
#17567=ADVANCED_FACE('',(#5123),#4693,.F.);
#17568=ADVANCED_FACE('',(#5124),#4694,.F.);
#17569=ADVANCED_FACE('',(#5125),#4695,.F.);
#17570=ADVANCED_FACE('',(#5126),#4696,.F.);
#17571=ADVANCED_FACE('',(#5127),#4697,.T.);
#17572=ADVANCED_FACE('',(#5128),#4698,.F.);
#17573=ADVANCED_FACE('',(#5129),#4699,.F.);
#17574=ADVANCED_FACE('',(#5130),#4700,.F.);
#17575=ADVANCED_FACE('',(#5131,#999),#137,.T.);
#17576=ADVANCED_FACE('',(#5132),#4701,.T.);
#17577=ADVANCED_FACE('',(#5133),#4702,.F.);
#17578=ADVANCED_FACE('',(#5134),#4703,.T.);
#17579=ADVANCED_FACE('',(#5135),#138,.T.);
#17580=ADVANCED_FACE('',(#5136),#4704,.F.);
#17581=ADVANCED_FACE('',(#5137),#4705,.F.);
#17582=ADVANCED_FACE('',(#5138),#4706,.F.);
#17583=ADVANCED_FACE('',(#5139),#4707,.F.);
#17584=ADVANCED_FACE('',(#5140),#4708,.T.);
#17585=ADVANCED_FACE('',(#5141),#4709,.F.);
#17586=ADVANCED_FACE('',(#5142),#4710,.F.);
#17587=ADVANCED_FACE('',(#5143),#139,.T.);
#17588=ADVANCED_FACE('',(#5144),#4711,.T.);
#17589=ADVANCED_FACE('',(#5145),#4712,.T.);
#17590=ADVANCED_FACE('',(#5146),#4713,.T.);
#17591=ADVANCED_FACE('',(#5147),#4714,.T.);
#17592=ADVANCED_FACE('',(#5148),#4715,.T.);
#17593=ADVANCED_FACE('',(#5149),#4716,.T.);
#17594=ADVANCED_FACE('',(#5150),#4717,.T.);
#17595=ADVANCED_FACE('',(#5151),#4718,.F.);
#17596=ADVANCED_FACE('',(#5152),#140,.T.);
#17597=ADVANCED_FACE('',(#5153),#141,.F.);
#17598=ADVANCED_FACE('',(#5154),#4719,.F.);
#17599=ADVANCED_FACE('',(#5155),#142,.T.);
#17600=ADVANCED_FACE('',(#5156),#4720,.T.);
#17601=ADVANCED_FACE('',(#5157),#4721,.T.);
#17602=ADVANCED_FACE('',(#5158),#143,.F.);
#17603=ADVANCED_FACE('',(#5159),#4722,.F.);
#17604=ADVANCED_FACE('',(#5160),#4723,.F.);
#17605=ADVANCED_FACE('',(#5161),#144,.F.);
#17606=ADVANCED_FACE('',(#5162),#190,.T.);
#17607=ADVANCED_FACE('',(#5163),#191,.T.);
#17608=ADVANCED_FACE('',(#5164),#192,.T.);
#17609=ADVANCED_FACE('',(#5165),#193,.F.);
#17610=ADVANCED_FACE('',(#5166),#194,.F.);
#17611=ADVANCED_FACE('',(#5167),#195,.T.);
#17612=ADVANCED_FACE('',(#5168),#196,.T.);
#17613=ADVANCED_FACE('',(#5169),#197,.T.);
#17614=ADVANCED_FACE('',(#5170),#198,.T.);
#17615=ADVANCED_FACE('',(#5171),#199,.T.);
#17616=ADVANCED_FACE('',(#5172),#200,.T.);
#17617=ADVANCED_FACE('',(#5173),#436,.T.);
#17618=ADVANCED_FACE('',(#5174),#437,.T.);
#17619=ADVANCED_FACE('',(#5175),#438,.T.);
#17620=ADVANCED_FACE('',(#5176),#439,.T.);
#17621=ADVANCED_FACE('',(#5177),#440,.T.);
#17622=ADVANCED_FACE('',(#5178),#441,.T.);
#17623=ADVANCED_FACE('',(#5179),#442,.T.);
#17624=ADVANCED_FACE('',(#5180),#443,.T.);
#17625=ADVANCED_FACE('',(#5181),#444,.T.);
#17626=ADVANCED_FACE('',(#5182),#445,.T.);
#17627=ADVANCED_FACE('',(#5183),#446,.T.);
#17628=ADVANCED_FACE('',(#5184),#447,.T.);
#17629=ADVANCED_FACE('',(#5185),#448,.T.);
#17630=ADVANCED_FACE('',(#5186),#449,.F.);
#17631=ADVANCED_FACE('',(#5187),#4724,.F.);
#17632=ADVANCED_FACE('',(#5188),#450,.F.);
#17633=ADVANCED_FACE('',(#5189),#451,.T.);
#17634=ADVANCED_FACE('',(#5190),#452,.T.);
#17635=ADVANCED_FACE('',(#5191),#453,.T.);
#17636=ADVANCED_FACE('',(#5192),#454,.T.);
#17637=ADVANCED_FACE('',(#5193),#455,.T.);
#17638=ADVANCED_FACE('',(#5194),#456,.T.);
#17639=ADVANCED_FACE('',(#5195),#457,.F.);
#17640=ADVANCED_FACE('',(#5196),#4725,.F.);
#17641=ADVANCED_FACE('',(#5197),#458,.F.);
#17642=ADVANCED_FACE('',(#5198),#459,.T.);
#17643=ADVANCED_FACE('',(#5199),#460,.T.);
#17644=ADVANCED_FACE('',(#5200),#461,.T.);
#17645=ADVANCED_FACE('',(#5201),#462,.T.);
#17646=ADVANCED_FACE('',(#5202),#463,.T.);
#17647=ADVANCED_FACE('',(#5203),#464,.T.);
#17648=ADVANCED_FACE('',(#5204),#465,.F.);
#17649=ADVANCED_FACE('',(#5205),#4726,.F.);
#17650=ADVANCED_FACE('',(#5206),#466,.F.);
#17651=ADVANCED_FACE('',(#5207),#467,.T.);
#17652=ADVANCED_FACE('',(#5208),#468,.T.);
#17653=ADVANCED_FACE('',(#5209),#469,.T.);
#17654=ADVANCED_FACE('',(#5210),#470,.T.);
#17655=ADVANCED_FACE('',(#5211),#471,.T.);
#17656=ADVANCED_FACE('',(#5212),#472,.T.);
#17657=ADVANCED_FACE('',(#5213),#473,.T.);
#17658=ADVANCED_FACE('',(#5214),#474,.F.);
#17659=ADVANCED_FACE('',(#5215),#4727,.F.);
#17660=ADVANCED_FACE('',(#5216),#475,.F.);
#17661=ADVANCED_FACE('',(#5217),#4728,.F.);
#17662=ADVANCED_FACE('',(#5218),#476,.F.);
#17663=ADVANCED_FACE('',(#5219),#4729,.F.);
#17664=ADVANCED_FACE('',(#5220),#4730,.F.);
#17665=ADVANCED_FACE('',(#5221),#4731,.F.);
#17666=ADVANCED_FACE('',(#5222),#477,.F.);
#17667=ADVANCED_FACE('',(#5223),#4732,.F.);
#17668=ADVANCED_FACE('',(#5224),#4733,.F.);
#17669=ADVANCED_FACE('',(#5225),#4734,.F.);
#17670=ADVANCED_FACE('',(#5226),#478,.F.);
#17671=ADVANCED_FACE('',(#5227),#4735,.F.);
#17672=ADVANCED_FACE('',(#5228),#4736,.F.);
#17673=ADVANCED_FACE('',(#5229),#479,.F.);
#17674=ADVANCED_FACE('',(#5230),#4737,.F.);
#17675=ADVANCED_FACE('',(#5231),#4738,.F.);
#17676=ADVANCED_FACE('',(#5232),#480,.F.);
#17677=ADVANCED_FACE('',(#5233),#481,.F.);
#17678=ADVANCED_FACE('',(#5234),#482,.F.);
#17679=ADVANCED_FACE('',(#5235),#483,.F.);
#17680=ADVANCED_FACE('',(#5236),#484,.F.);
#17681=ADVANCED_FACE('',(#5237),#485,.F.);
#17682=ADVANCED_FACE('',(#5238),#486,.F.);
#17683=ADVANCED_FACE('',(#5239),#487,.F.);
#17684=ADVANCED_FACE('',(#5240),#488,.F.);
#17685=ADVANCED_FACE('',(#5241),#489,.F.);
#17686=ADVANCED_FACE('',(#5242),#490,.F.);
#17687=ADVANCED_FACE('',(#5243),#491,.F.);
#17688=ADVANCED_FACE('',(#5244),#4739,.T.);
#17689=ADVANCED_FACE('',(#5245),#4740,.T.);
#17690=ADVANCED_FACE('',(#5246,#1000),#492,.F.);
#17691=ADVANCED_FACE('',(#5247),#4741,.T.);
#17692=ADVANCED_FACE('',(#5248,#1001),#493,.T.);
#17693=ADVANCED_FACE('',(#5249,#1002),#494,.T.);
#17694=ADVANCED_FACE('',(#5250),#4742,.T.);
#17695=ADVANCED_FACE('',(#5251,#1003),#495,.T.);
#17696=ADVANCED_FACE('',(#5252),#496,.T.);
#17697=ADVANCED_FACE('',(#5253),#4743,.T.);
#17698=ADVANCED_FACE('',(#5254),#497,.T.);
#17699=ADVANCED_FACE('',(#5255),#498,.T.);
#17700=ADVANCED_FACE('',(#5256),#4744,.T.);
#17701=ADVANCED_FACE('',(#5257),#499,.T.);
#17702=ADVANCED_FACE('',(#5258),#500,.T.);
#17703=ADVANCED_FACE('',(#5259),#4745,.T.);
#17704=ADVANCED_FACE('',(#5260),#501,.T.);
#17705=ADVANCED_FACE('',(#5261),#502,.T.);
#17706=ADVANCED_FACE('',(#5262),#4746,.T.);
#17707=ADVANCED_FACE('',(#5263),#503,.T.);
#17708=ADVANCED_FACE('',(#5264,#1004),#504,.T.);
#17709=ADVANCED_FACE('',(#5265,#1005),#505,.F.);
#17710=ADVANCED_FACE('',(#5266,#1006),#95,.T.);
#17711=ADVANCED_FACE('',(#5267,#1007),#96,.T.);
#17712=ADVANCED_FACE('',(#5268),#4747,.T.);
#17713=ADVANCED_FACE('',(#5269),#506,.T.);
#17714=ADVANCED_FACE('',(#5270),#4748,.T.);
#17715=ADVANCED_FACE('',(#5271),#507,.T.);
#17716=ADVANCED_FACE('',(#5272),#4749,.T.);
#17717=ADVANCED_FACE('',(#5273),#508,.T.);
#17718=ADVANCED_FACE('',(#5274),#4750,.T.);
#17719=ADVANCED_FACE('',(#5275),#509,.T.);
#17720=ADVANCED_FACE('',(#5276),#201,.T.);
#17721=ADVANCED_FACE('',(#5277),#202,.T.);
#17722=ADVANCED_FACE('',(#5278),#203,.T.);
#17723=ADVANCED_FACE('',(#5279),#204,.T.);
#17724=ADVANCED_FACE('',(#5280),#510,.T.);
#17725=ADVANCED_FACE('',(#5281),#205,.F.);
#17726=ADVANCED_FACE('',(#5282),#206,.F.);
#17727=ADVANCED_FACE('',(#5283),#511,.T.);
#17728=ADVANCED_FACE('',(#5284),#207,.F.);
#17729=ADVANCED_FACE('',(#5285),#208,.F.);
#17730=ADVANCED_FACE('',(#5286),#512,.T.);
#17731=ADVANCED_FACE('',(#5287),#209,.F.);
#17732=ADVANCED_FACE('',(#5288),#210,.F.);
#17733=ADVANCED_FACE('',(#5289),#513,.T.);
#17734=ADVANCED_FACE('',(#5290),#211,.F.);
#17735=ADVANCED_FACE('',(#5291),#212,.T.);
#17736=ADVANCED_FACE('',(#5292),#213,.T.);
#17737=ADVANCED_FACE('',(#5293),#214,.T.);
#17738=ADVANCED_FACE('',(#5294),#215,.T.);
#17739=ADVANCED_FACE('',(#5295),#514,.T.);
#17740=ADVANCED_FACE('',(#5296),#216,.T.);
#17741=ADVANCED_FACE('',(#5297),#217,.T.);
#17742=ADVANCED_FACE('',(#5298),#515,.T.);
#17743=ADVANCED_FACE('',(#5299),#218,.F.);
#17744=ADVANCED_FACE('',(#5300),#219,.F.);
#17745=ADVANCED_FACE('',(#5301),#516,.T.);
#17746=ADVANCED_FACE('',(#5302),#220,.F.);
#17747=ADVANCED_FACE('',(#5303),#221,.F.);
#17748=ADVANCED_FACE('',(#5304),#517,.T.);
#17749=ADVANCED_FACE('',(#5305),#222,.F.);
#17750=ADVANCED_FACE('',(#5306),#223,.F.);
#17751=ADVANCED_FACE('',(#5307),#224,.F.);
#17752=ADVANCED_FACE('',(#5308),#225,.T.);
#17753=ADVANCED_FACE('',(#5309),#226,.T.);
#17754=ADVANCED_FACE('',(#5310),#227,.T.);
#17755=ADVANCED_FACE('',(#5311),#145,.T.);
#17756=ADVANCED_FACE('',(#5312),#518,.F.);
#17757=ADVANCED_FACE('',(#5313),#248,.F.);
#17758=ADVANCED_FACE('',(#5314),#249,.F.);
#17759=ADVANCED_FACE('',(#5315),#519,.F.);
#17760=ADVANCED_FACE('',(#5316),#250,.F.);
#17761=ADVANCED_FACE('',(#5317),#251,.F.);
#17762=ADVANCED_FACE('',(#5318),#520,.F.);
#17763=ADVANCED_FACE('',(#5319),#252,.F.);
#17764=ADVANCED_FACE('',(#5320),#253,.F.);
#17765=ADVANCED_FACE('',(#5321),#521,.F.);
#17766=ADVANCED_FACE('',(#5322),#254,.F.);
#17767=ADVANCED_FACE('',(#5323),#228,.T.);
#17768=ADVANCED_FACE('',(#5324),#255,.F.);
#17769=ADVANCED_FACE('',(#5325),#229,.T.);
#17770=ADVANCED_FACE('',(#5326),#230,.T.);
#17771=ADVANCED_FACE('',(#5327),#522,.T.);
#17772=ADVANCED_FACE('',(#5328),#231,.T.);
#17773=ADVANCED_FACE('',(#5329),#232,.T.);
#17774=ADVANCED_FACE('',(#5330),#523,.T.);
#17775=ADVANCED_FACE('',(#5331),#233,.F.);
#17776=ADVANCED_FACE('',(#5332),#234,.F.);
#17777=ADVANCED_FACE('',(#5333),#524,.T.);
#17778=ADVANCED_FACE('',(#5334),#235,.F.);
#17779=ADVANCED_FACE('',(#5335),#236,.F.);
#17780=ADVANCED_FACE('',(#5336),#525,.T.);
#17781=ADVANCED_FACE('',(#5337),#237,.F.);
#17782=ADVANCED_FACE('',(#5338),#238,.F.);
#17783=ADVANCED_FACE('',(#5339),#239,.F.);
#17784=ADVANCED_FACE('',(#5340,#1008),#526,.F.);
#17785=ADVANCED_FACE('',(#5341),#146,.T.);
#17786=ADVANCED_FACE('',(#5342),#147,.T.);
#17787=ADVANCED_FACE('',(#5343),#148,.T.);
#17788=ADVANCED_FACE('',(#5344),#149,.T.);
#17789=ADVANCED_FACE('',(#5345),#150,.T.);
#17790=ADVANCED_FACE('',(#5346),#151,.T.);
#17791=ADVANCED_FACE('',(#5347),#152,.T.);
#17792=ADVANCED_FACE('',(#5348),#153,.T.);
#17793=ADVANCED_FACE('',(#5349),#154,.T.);
#17794=ADVANCED_FACE('',(#5350),#155,.T.);
#17795=ADVANCED_FACE('',(#5351),#156,.T.);
#17796=ADVANCED_FACE('',(#5352),#157,.T.);
#17797=ADVANCED_FACE('',(#5353),#158,.T.);
#17798=ADVANCED_FACE('',(#5354),#159,.T.);
#17799=ADVANCED_FACE('',(#5355),#160,.T.);
#17800=ADVANCED_FACE('',(#5356),#527,.T.);
#17801=ADVANCED_FACE('',(#5357,#1009,#1010),#528,.T.);
#17802=ADVANCED_FACE('',(#5358),#4751,.T.);
#17803=ADVANCED_FACE('',(#5359),#529,.T.);
#17804=ADVANCED_FACE('',(#5360),#4752,.T.);
#17805=ADVANCED_FACE('',(#5361),#4753,.T.);
#17806=ADVANCED_FACE('',(#5362),#4754,.T.);
#17807=ADVANCED_FACE('',(#5363),#530,.T.);
#17808=ADVANCED_FACE('',(#5364),#256,.F.);
#17809=ADVANCED_FACE('',(#5365),#257,.F.);
#17810=ADVANCED_FACE('',(#5366),#258,.F.);
#17811=ADVANCED_FACE('',(#5367),#259,.T.);
#17812=ADVANCED_FACE('',(#5368),#260,.T.);
#17813=ADVANCED_FACE('',(#5369),#261,.T.);
#17814=ADVANCED_FACE('',(#5370),#262,.T.);
#17815=ADVANCED_FACE('',(#5371),#263,.T.);
#17816=ADVANCED_FACE('',(#5372),#264,.T.);
#17817=ADVANCED_FACE('',(#5373),#265,.F.);
#17818=ADVANCED_FACE('',(#5374),#266,.F.);
#17819=ADVANCED_FACE('',(#5375),#267,.F.);
#17820=ADVANCED_FACE('',(#5376,#1011),#531,.T.);
#17821=ADVANCED_FACE('',(#5377),#532,.F.);
#17822=ADVANCED_FACE('',(#5378),#533,.F.);
#17823=ADVANCED_FACE('',(#5379),#4755,.T.);
#17824=ADVANCED_FACE('',(#5380),#4756,.T.);
#17825=ADVANCED_FACE('',(#5381),#4757,.T.);
#17826=ADVANCED_FACE('',(#5382),#4758,.T.);
#17827=ADVANCED_FACE('',(#5383),#161,.T.);
#17828=ADVANCED_FACE('',(#5384),#534,.T.);
#17829=ADVANCED_FACE('',(#5385),#535,.T.);
#17830=ADVANCED_FACE('',(#5386),#536,.T.);
#17831=ADVANCED_FACE('',(#5387),#162,.T.);
#17832=ADVANCED_FACE('',(#5388),#163,.T.);
#17833=ADVANCED_FACE('',(#5389),#164,.T.);
#17834=ADVANCED_FACE('',(#5390),#537,.T.);
#17835=ADVANCED_FACE('',(#5391),#538,.T.);
#17836=ADVANCED_FACE('',(#5392),#539,.T.);
#17837=ADVANCED_FACE('',(#5393),#165,.T.);
#17838=ADVANCED_FACE('',(#5394),#166,.T.);
#17839=ADVANCED_FACE('',(#5395),#540,.T.);
#17840=ADVANCED_FACE('',(#5396),#541,.T.);
#17841=ADVANCED_FACE('',(#5397),#542,.T.);
#17842=ADVANCED_FACE('',(#5398),#167,.T.);
#17843=ADVANCED_FACE('',(#5399),#168,.T.);
#17844=ADVANCED_FACE('',(#5400),#169,.T.);
#17845=ADVANCED_FACE('',(#5401),#543,.T.);
#17846=ADVANCED_FACE('',(#5402),#544,.T.);
#17847=ADVANCED_FACE('',(#5403),#545,.T.);
#17848=ADVANCED_FACE('',(#5404),#170,.T.);
#17849=ADVANCED_FACE('',(#5405),#171,.T.);
#17850=ADVANCED_FACE('',(#5406),#546,.F.);
#17851=ADVANCED_FACE('',(#5407),#547,.F.);
#17852=ADVANCED_FACE('',(#5408),#548,.F.);
#17853=ADVANCED_FACE('',(#5409),#549,.F.);
#17854=ADVANCED_FACE('',(#5410),#550,.F.);
#17855=ADVANCED_FACE('',(#5411),#551,.F.);
#17856=ADVANCED_FACE('',(#5412),#552,.F.);
#17857=ADVANCED_FACE('',(#5413),#553,.F.);
#17858=ADVANCED_FACE('',(#5414),#554,.F.);
#17859=ADVANCED_FACE('',(#5415),#555,.F.);
#17860=ADVANCED_FACE('',(#5416),#556,.F.);
#17861=ADVANCED_FACE('',(#5417),#557,.F.);
#17862=ADVANCED_FACE('',(#5418),#4759,.T.);
#17863=ADVANCED_FACE('',(#5419),#4760,.T.);
#17864=ADVANCED_FACE('',(#5420,#1012),#558,.F.);
#17865=ADVANCED_FACE('',(#5421),#559,.F.);
#17866=ADVANCED_FACE('',(#5422),#4761,.T.);
#17867=ADVANCED_FACE('',(#5423),#4762,.T.);
#17868=ADVANCED_FACE('',(#5424),#4763,.T.);
#17869=ADVANCED_FACE('',(#5425),#4764,.T.);
#17870=ADVANCED_FACE('',(#5426,#1013),#560,.T.);
#17871=ADVANCED_FACE('',(#5427),#4765,.T.);
#17872=ADVANCED_FACE('',(#5428,#1014),#561,.T.);
#17873=ADVANCED_FACE('',(#5429,#1015),#562,.T.);
#17874=ADVANCED_FACE('',(#5430),#563,.T.);
#17875=ADVANCED_FACE('',(#5431),#564,.T.);
#17876=ADVANCED_FACE('',(#5432),#565,.F.);
#17877=ADVANCED_FACE('',(#5433),#4766,.F.);
#17878=ADVANCED_FACE('',(#5434),#566,.T.);
#17879=ADVANCED_FACE('',(#5435,#1016),#567,.F.);
#17880=ADVANCED_FACE('',(#5436),#568,.F.);
#17881=ADVANCED_FACE('',(#5437),#569,.F.);
#17882=ADVANCED_FACE('',(#5438),#570,.F.);
#17883=ADVANCED_FACE('',(#5439),#571,.F.);
#17884=ADVANCED_FACE('',(#5440),#572,.T.);
#17885=ADVANCED_FACE('',(#5441),#573,.F.);
#17886=ADVANCED_FACE('',(#5442),#4767,.F.);
#17887=ADVANCED_FACE('',(#5443),#574,.T.);
#17888=ADVANCED_FACE('',(#5444,#1017),#575,.F.);
#17889=ADVANCED_FACE('',(#5445),#576,.T.);
#17890=ADVANCED_FACE('',(#5446),#577,.F.);
#17891=ADVANCED_FACE('',(#5447),#4768,.F.);
#17892=ADVANCED_FACE('',(#5448),#578,.T.);
#17893=ADVANCED_FACE('',(#5449,#1018),#579,.F.);
#17894=ADVANCED_FACE('',(#5450),#4769,.F.);
#17895=ADVANCED_FACE('',(#5451,#1019),#580,.F.);
#17896=ADVANCED_FACE('',(#5452),#581,.T.);
#17897=ADVANCED_FACE('',(#5453),#582,.F.);
#17898=ADVANCED_FACE('',(#5454),#583,.F.);
#17899=ADVANCED_FACE('',(#5455),#584,.F.);
#17900=ADVANCED_FACE('',(#5456,#1020),#585,.T.);
#17901=ADVANCED_FACE('',(#5457,#1021),#586,.T.);
#17902=ADVANCED_FACE('',(#5458),#4770,.T.);
#17903=ADVANCED_FACE('',(#5459),#587,.F.);
#17904=ADVANCED_FACE('',(#5460),#4771,.T.);
#17905=ADVANCED_FACE('',(#5461),#588,.F.);
#17906=ADVANCED_FACE('',(#5462),#589,.F.);
#17907=ADVANCED_FACE('',(#5463),#590,.F.);
#17908=ADVANCED_FACE('',(#5464),#4772,.T.);
#17909=ADVANCED_FACE('',(#5465),#591,.F.);
#17910=ADVANCED_FACE('',(#5466,#1022),#592,.T.);
#17911=ADVANCED_FACE('',(#5467),#4773,.T.);
#17912=ADVANCED_FACE('',(#5468),#593,.F.);
#17913=ADVANCED_FACE('',(#5469),#4774,.T.);
#17914=ADVANCED_FACE('',(#5470),#594,.F.);
#17915=ADVANCED_FACE('',(#5471),#595,.F.);
#17916=ADVANCED_FACE('',(#5472),#596,.F.);
#17917=ADVANCED_FACE('',(#5473),#4775,.T.);
#17918=ADVANCED_FACE('',(#5474),#597,.F.);
#17919=ADVANCED_FACE('',(#5475,#1023),#598,.T.);
#17920=ADVANCED_FACE('',(#5476),#4776,.T.);
#17921=ADVANCED_FACE('',(#5477),#599,.F.);
#17922=ADVANCED_FACE('',(#5478),#4777,.T.);
#17923=ADVANCED_FACE('',(#5479),#600,.F.);
#17924=ADVANCED_FACE('',(#5480),#601,.F.);
#17925=ADVANCED_FACE('',(#5481),#602,.F.);
#17926=ADVANCED_FACE('',(#5482),#4778,.T.);
#17927=ADVANCED_FACE('',(#5483),#603,.F.);
#17928=ADVANCED_FACE('',(#5484,#1024),#604,.T.);
#17929=ADVANCED_FACE('',(#5485),#4779,.T.);
#17930=ADVANCED_FACE('',(#5486),#605,.F.);
#17931=ADVANCED_FACE('',(#5487),#4780,.T.);
#17932=ADVANCED_FACE('',(#5488),#606,.F.);
#17933=ADVANCED_FACE('',(#5489),#607,.F.);
#17934=ADVANCED_FACE('',(#5490),#608,.F.);
#17935=ADVANCED_FACE('',(#5491),#4781,.T.);
#17936=ADVANCED_FACE('',(#5492),#609,.F.);
#17937=ADVANCED_FACE('',(#5493),#610,.F.);
#17938=ADVANCED_FACE('',(#5494),#611,.F.);
#17939=ADVANCED_FACE('',(#5495),#612,.F.);
#17940=ADVANCED_FACE('',(#5496),#613,.F.);
#17941=ADVANCED_FACE('',(#5497),#614,.F.);
#17942=ADVANCED_FACE('',(#5498),#615,.F.);
#17943=ADVANCED_FACE('',(#5499,#1025),#616,.T.);
#17944=ADVANCED_FACE('',(#5500,#1026),#617,.T.);
#17945=ADVANCED_FACE('',(#5501),#618,.F.);
#17946=ADVANCED_FACE('',(#5502),#619,.F.);
#17947=ADVANCED_FACE('',(#5503),#620,.F.);
#17948=ADVANCED_FACE('',(#5504),#621,.T.);
#17949=ADVANCED_FACE('',(#5505),#622,.F.);
#17950=ADVANCED_FACE('',(#5506),#623,.F.);
#17951=ADVANCED_FACE('',(#5507),#624,.F.);
#17952=ADVANCED_FACE('',(#5508),#625,.F.);
#17953=ADVANCED_FACE('',(#5509),#626,.F.);
#17954=ADVANCED_FACE('',(#5510),#627,.F.);
#17955=ADVANCED_FACE('',(#5511),#628,.F.);
#17956=ADVANCED_FACE('',(#5512),#629,.T.);
#17957=ADVANCED_FACE('',(#5513),#630,.F.);
#17958=ADVANCED_FACE('',(#5514),#631,.F.);
#17959=ADVANCED_FACE('',(#5515),#632,.F.);
#17960=ADVANCED_FACE('',(#5516),#633,.T.);
#17961=ADVANCED_FACE('',(#5517),#634,.F.);
#17962=ADVANCED_FACE('',(#5518),#635,.F.);
#17963=ADVANCED_FACE('',(#5519),#636,.F.);
#17964=ADVANCED_FACE('',(#5520),#637,.T.);
#17965=ADVANCED_FACE('',(#5521),#638,.F.);
#17966=ADVANCED_FACE('',(#5522),#639,.F.);
#17967=ADVANCED_FACE('',(#5523),#640,.F.);
#17968=ADVANCED_FACE('',(#5524),#641,.T.);
#17969=ADVANCED_FACE('',(#5525,#1027),#642,.T.);
#17970=ADVANCED_FACE('',(#5526),#643,.T.);
#17971=ADVANCED_FACE('',(#5527),#644,.T.);
#17972=ADVANCED_FACE('',(#5528),#4782,.T.);
#17973=ADVANCED_FACE('',(#5529),#645,.T.);
#17974=ADVANCED_FACE('',(#5530),#4783,.T.);
#17975=ADVANCED_FACE('',(#5531),#646,.T.);
#17976=ADVANCED_FACE('',(#5532),#4784,.T.);
#17977=ADVANCED_FACE('',(#5533),#647,.T.);
#17978=ADVANCED_FACE('',(#5534),#648,.T.);
#17979=ADVANCED_FACE('',(#5535),#4785,.T.);
#17980=ADVANCED_FACE('',(#5536),#649,.T.);
#17981=ADVANCED_FACE('',(#5537),#4786,.T.);
#17982=ADVANCED_FACE('',(#5538),#650,.T.);
#17983=ADVANCED_FACE('',(#5539),#4787,.T.);
#17984=ADVANCED_FACE('',(#5540),#651,.T.);
#17985=ADVANCED_FACE('',(#5541),#4788,.T.);
#17986=ADVANCED_FACE('',(#5542,#1028),#652,.F.);
#17987=ADVANCED_FACE('',(#5543),#653,.T.);
#17988=ADVANCED_FACE('',(#5544),#654,.T.);
#17989=ADVANCED_FACE('',(#5545,#1029),#655,.T.);
#17990=ADVANCED_FACE('',(#5546),#656,.T.);
#17991=ADVANCED_FACE('',(#5547),#4789,.T.);
#17992=ADVANCED_FACE('',(#5548),#657,.F.);
#17993=ADVANCED_FACE('',(#5549),#658,.F.);
#17994=ADVANCED_FACE('',(#5550),#659,.F.);
#17995=ADVANCED_FACE('',(#5551),#660,.F.);
#17996=ADVANCED_FACE('',(#5552),#661,.F.);
#17997=ADVANCED_FACE('',(#5553),#662,.F.);
#17998=ADVANCED_FACE('',(#5554),#4790,.F.);
#17999=ADVANCED_FACE('',(#5555),#663,.T.);
#18000=ADVANCED_FACE('',(#5556,#1030),#664,.T.);
#18001=ADVANCED_FACE('',(#5557,#1031),#665,.T.);
#18002=ADVANCED_FACE('',(#5558,#1032),#666,.T.);
#18003=ADVANCED_FACE('',(#5559,#1033),#667,.T.);
#18004=ADVANCED_FACE('',(#5560,#1034),#668,.T.);
#18005=ADVANCED_FACE('',(#5561),#4791,.T.);
#18006=ADVANCED_FACE('',(#5562),#669,.T.);
#18007=ADVANCED_FACE('',(#5563),#670,.F.);
#18008=ADVANCED_FACE('',(#5564),#671,.T.);
#18009=ADVANCED_FACE('',(#5565),#672,.T.);
#18010=ADVANCED_FACE('',(#5566),#673,.T.);
#18011=ADVANCED_FACE('',(#5567),#674,.T.);
#18012=ADVANCED_FACE('',(#5568),#675,.T.);
#18013=ADVANCED_FACE('',(#5569),#676,.T.);
#18014=ADVANCED_FACE('',(#5570),#677,.T.);
#18015=ADVANCED_FACE('',(#5571),#678,.T.);
#18016=ADVANCED_FACE('',(#5572),#679,.T.);
#18017=ADVANCED_FACE('',(#5573),#680,.T.);
#18018=ADVANCED_FACE('',(#5574),#681,.T.);
#18019=ADVANCED_FACE('',(#5575),#682,.T.);
#18020=ADVANCED_FACE('',(#5576),#683,.T.);
#18021=ADVANCED_FACE('',(#5577),#684,.T.);
#18022=ADVANCED_FACE('',(#5578),#685,.T.);
#18023=ADVANCED_FACE('',(#5579),#686,.F.);
#18024=ADVANCED_FACE('',(#5580),#687,.F.);
#18025=ADVANCED_FACE('',(#5581),#688,.F.);
#18026=ADVANCED_FACE('',(#5582),#689,.F.);
#18027=ADVANCED_FACE('',(#5583),#690,.F.);
#18028=ADVANCED_FACE('',(#5584),#691,.F.);
#18029=ADVANCED_FACE('',(#5585),#692,.T.);
#18030=ADVANCED_FACE('',(#5586),#4792,.T.);
#18031=ADVANCED_FACE('',(#5587,#1035),#693,.F.);
#18032=ADVANCED_FACE('',(#5588),#4793,.T.);
#18033=ADVANCED_FACE('',(#5589),#694,.T.);
#18034=ADVANCED_FACE('',(#5590),#695,.T.);
#18035=ADVANCED_FACE('',(#5591),#696,.T.);
#18036=ADVANCED_FACE('',(#5592),#697,.T.);
#18037=ADVANCED_FACE('',(#5593),#698,.T.);
#18038=ADVANCED_FACE('',(#5594,#1036),#699,.F.);
#18039=ADVANCED_FACE('',(#5595),#700,.F.);
#18040=ADVANCED_FACE('',(#5596),#701,.F.);
#18041=ADVANCED_FACE('',(#5597),#702,.F.);
#18042=ADVANCED_FACE('',(#5598),#703,.F.);
#18043=ADVANCED_FACE('',(#5599),#704,.F.);
#18044=ADVANCED_FACE('',(#5600),#705,.F.);
#18045=ADVANCED_FACE('',(#5601),#706,.F.);
#18046=ADVANCED_FACE('',(#5602),#707,.F.);
#18047=ADVANCED_FACE('',(#5603),#708,.F.);
#18048=ADVANCED_FACE('',(#5604),#709,.T.);
#18049=ADVANCED_FACE('',(#5605),#4794,.F.);
#18050=ADVANCED_FACE('',(#5606),#710,.T.);
#18051=ADVANCED_FACE('',(#5607),#711,.F.);
#18052=ADVANCED_FACE('',(#5608),#712,.F.);
#18053=ADVANCED_FACE('',(#5609),#713,.F.);
#18054=ADVANCED_FACE('',(#5610),#714,.F.);
#18055=ADVANCED_FACE('',(#5611),#715,.F.);
#18056=ADVANCED_FACE('',(#5612),#716,.F.);
#18057=ADVANCED_FACE('',(#5613),#4795,.F.);
#18058=ADVANCED_FACE('',(#5614),#717,.T.);
#18059=ADVANCED_FACE('',(#5615),#718,.F.);
#18060=ADVANCED_FACE('',(#5616),#719,.F.);
#18061=ADVANCED_FACE('',(#5617),#720,.F.);
#18062=ADVANCED_FACE('',(#5618),#721,.F.);
#18063=ADVANCED_FACE('',(#5619),#722,.F.);
#18064=ADVANCED_FACE('',(#5620),#723,.F.);
#18065=ADVANCED_FACE('',(#5621),#4796,.T.);
#18066=ADVANCED_FACE('',(#5622),#4797,.T.);
#18067=ADVANCED_FACE('',(#5623),#4798,.T.);
#18068=ADVANCED_FACE('',(#5624),#724,.T.);
#18069=ADVANCED_FACE('',(#5625),#4799,.T.);
#18070=ADVANCED_FACE('',(#5626,#1037),#725,.T.);
#18071=ADVANCED_FACE('',(#5627),#4800,.T.);
#18072=ADVANCED_FACE('',(#5628),#726,.T.);
#18073=ADVANCED_FACE('',(#5629),#4801,.T.);
#18074=ADVANCED_FACE('',(#5630),#4802,.T.);
#18075=ADVANCED_FACE('',(#5631),#4803,.T.);
#18076=ADVANCED_FACE('',(#5632),#727,.F.);
#18077=ADVANCED_FACE('',(#5633),#728,.T.);
#18078=ADVANCED_FACE('',(#5634),#240,.T.);
#18079=ADVANCED_FACE('',(#5635),#729,.F.);
#18080=ADVANCED_FACE('',(#5636),#730,.T.);
#18081=ADVANCED_FACE('',(#5637),#4804,.F.);
#18082=ADVANCED_FACE('',(#5638),#731,.T.);
#18083=ADVANCED_FACE('',(#5639),#4805,.T.);
#18084=ADVANCED_FACE('',(#5640),#732,.F.);
#18085=ADVANCED_FACE('',(#5641),#733,.F.);
#18086=ADVANCED_FACE('',(#5642),#734,.F.);
#18087=ADVANCED_FACE('',(#5643),#735,.F.);
#18088=ADVANCED_FACE('',(#5644),#736,.F.);
#18089=ADVANCED_FACE('',(#5645),#737,.F.);
#18090=ADVANCED_FACE('',(#5646),#241,.T.);
#18091=ADVANCED_FACE('',(#5647),#738,.T.);
#18092=ADVANCED_FACE('',(#5648),#4806,.F.);
#18093=ADVANCED_FACE('',(#5649),#739,.T.);
#18094=ADVANCED_FACE('',(#5650),#740,.F.);
#18095=ADVANCED_FACE('',(#5651),#741,.F.);
#18096=ADVANCED_FACE('',(#5652),#742,.F.);
#18097=ADVANCED_FACE('',(#5653),#743,.F.);
#18098=ADVANCED_FACE('',(#5654),#744,.F.);
#18099=ADVANCED_FACE('',(#5655),#745,.F.);
#18100=ADVANCED_FACE('',(#5656),#746,.F.);
#18101=ADVANCED_FACE('',(#5657),#747,.F.);
#18102=ADVANCED_FACE('',(#5658),#748,.F.);
#18103=ADVANCED_FACE('',(#5659),#749,.F.);
#18104=ADVANCED_FACE('',(#5660),#750,.F.);
#18105=ADVANCED_FACE('',(#5661),#751,.F.);
#18106=ADVANCED_FACE('',(#5662,#1038),#752,.T.);
#18107=ADVANCED_FACE('',(#5663),#753,.F.);
#18108=ADVANCED_FACE('',(#5664,#1039,#1040,#1041,#1042,#1043),#754,.F.);
#18109=ADVANCED_FACE('',(#5665),#755,.T.);
#18110=ADVANCED_FACE('',(#5666),#756,.T.);
#18111=ADVANCED_FACE('',(#5667),#757,.F.);
#18112=ADVANCED_FACE('',(#5668),#758,.T.);
#18113=ADVANCED_FACE('',(#5669),#759,.F.);
#18114=ADVANCED_FACE('',(#5670),#760,.F.);
#18115=ADVANCED_FACE('',(#5671),#761,.F.);
#18116=ADVANCED_FACE('',(#5672),#762,.F.);
#18117=ADVANCED_FACE('',(#5673),#763,.F.);
#18118=ADVANCED_FACE('',(#5674),#764,.F.);
#18119=ADVANCED_FACE('',(#5675),#765,.F.);
#18120=ADVANCED_FACE('',(#5676),#766,.F.);
#18121=ADVANCED_FACE('',(#5677),#767,.F.);
#18122=ADVANCED_FACE('',(#5678),#768,.F.);
#18123=ADVANCED_FACE('',(#5679),#769,.F.);
#18124=ADVANCED_FACE('',(#5680),#770,.F.);
#18125=ADVANCED_FACE('',(#5681,#1044),#771,.T.);
#18126=ADVANCED_FACE('',(#5682),#4807,.T.);
#18127=ADVANCED_FACE('',(#5683,#1045),#772,.F.);
#18128=ADVANCED_FACE('',(#5684),#242,.T.);
#18129=ADVANCED_FACE('',(#5685,#1046),#773,.T.);
#18130=ADVANCED_FACE('',(#5686),#4808,.T.);
#18131=ADVANCED_FACE('',(#5687),#243,.T.);
#18132=ADVANCED_FACE('',(#5688),#774,.F.);
#18133=ADVANCED_FACE('',(#5689),#4809,.T.);
#18134=ADVANCED_FACE('',(#5690),#775,.T.);
#18135=ADVANCED_FACE('',(#5691),#4810,.T.);
#18136=ADVANCED_FACE('',(#5692,#1047),#776,.T.);
#18137=ADVANCED_FACE('',(#5693),#4811,.T.);
#18138=ADVANCED_FACE('',(#5694,#1048),#777,.F.);
#18139=ADVANCED_FACE('',(#5695,#1049),#778,.T.);
#18140=ADVANCED_FACE('',(#5696),#779,.F.);
#18141=ADVANCED_FACE('',(#5697),#780,.F.);
#18142=ADVANCED_FACE('',(#5698),#781,.F.);
#18143=ADVANCED_FACE('',(#5699),#782,.F.);
#18144=ADVANCED_FACE('',(#5700),#783,.F.);
#18145=ADVANCED_FACE('',(#5701),#784,.F.);
#18146=ADVANCED_FACE('',(#5702),#785,.T.);
#18147=ADVANCED_FACE('',(#5703),#786,.T.);
#18148=ADVANCED_FACE('',(#5704),#787,.T.);
#18149=ADVANCED_FACE('',(#5705),#788,.T.);
#18150=ADVANCED_FACE('',(#5706),#789,.T.);
#18151=ADVANCED_FACE('',(#5707),#790,.T.);
#18152=ADVANCED_FACE('',(#5708),#791,.T.);
#18153=ADVANCED_FACE('',(#5709,#1050),#792,.T.);
#18154=ADVANCED_FACE('',(#5710),#793,.T.);
#18155=ADVANCED_FACE('',(#5711),#794,.T.);
#18156=ADVANCED_FACE('',(#5712),#795,.F.);
#18157=ADVANCED_FACE('',(#5713),#796,.F.);
#18158=ADVANCED_FACE('',(#5714),#797,.T.);
#18159=ADVANCED_FACE('',(#5715),#798,.F.);
#18160=ADVANCED_FACE('',(#5716),#4812,.T.);
#18161=ADVANCED_FACE('',(#5717),#799,.F.);
#18162=ADVANCED_FACE('',(#5718),#4813,.T.);
#18163=ADVANCED_FACE('',(#5719),#800,.T.);
#18164=ADVANCED_FACE('',(#5720),#801,.F.);
#18165=ADVANCED_FACE('',(#5721),#802,.F.);
#18166=ADVANCED_FACE('',(#5722),#803,.F.);
#18167=ADVANCED_FACE('',(#5723),#804,.T.);
#18168=ADVANCED_FACE('',(#5724),#4814,.F.);
#18169=ADVANCED_FACE('',(#5725,#1051),#805,.F.);
#18170=ADVANCED_FACE('',(#5726),#4815,.F.);
#18171=ADVANCED_FACE('',(#5727),#806,.T.);
#18172=ADVANCED_FACE('',(#5728,#1052),#807,.T.);
#18173=ADVANCED_FACE('',(#5729),#808,.F.);
#18174=ADVANCED_FACE('',(#5730),#809,.T.);
#18175=ADVANCED_FACE('',(#5731),#810,.F.);
#18176=ADVANCED_FACE('',(#5732),#811,.T.);
#18177=ADVANCED_FACE('',(#5733),#812,.T.);
#18178=ADVANCED_FACE('',(#5734),#813,.T.);
#18179=ADVANCED_FACE('',(#5735,#1053),#814,.T.);
#18180=ADVANCED_FACE('',(#5736),#815,.T.);
#18181=ADVANCED_FACE('',(#5737),#816,.T.);
#18182=ADVANCED_FACE('',(#5738),#817,.T.);
#18183=ADVANCED_FACE('',(#5739),#818,.F.);
#18184=ADVANCED_FACE('',(#5740),#819,.T.);
#18185=ADVANCED_FACE('',(#5741),#820,.F.);
#18186=ADVANCED_FACE('',(#5742),#821,.T.);
#18187=ADVANCED_FACE('',(#5743),#4816,.F.);
#18188=ADVANCED_FACE('',(#5744),#4817,.F.);
#18189=ADVANCED_FACE('',(#5745),#4818,.F.);
#18190=ADVANCED_FACE('',(#5746),#822,.T.);
#18191=ADVANCED_FACE('',(#5747),#823,.T.);
#18192=ADVANCED_FACE('',(#5748),#824,.T.);
#18193=ADVANCED_FACE('',(#5749),#825,.F.);
#18194=ADVANCED_FACE('',(#5750),#826,.T.);
#18195=ADVANCED_FACE('',(#5751),#827,.T.);
#18196=ADVANCED_FACE('',(#5752),#828,.T.);
#18197=ADVANCED_FACE('',(#5753),#4819,.F.);
#18198=ADVANCED_FACE('',(#5754),#172,.T.);
#18199=ADVANCED_FACE('',(#5755),#173,.T.);
#18200=ADVANCED_FACE('',(#5756),#174,.T.);
#18201=ADVANCED_FACE('',(#5757),#175,.T.);
#18202=ADVANCED_FACE('',(#5758,#1054),#829,.T.);
#18203=ADVANCED_FACE('',(#5759),#830,.T.);
#18204=ADVANCED_FACE('',(#5760),#831,.T.);
#18205=ADVANCED_FACE('',(#5761),#832,.T.);
#18206=ADVANCED_FACE('',(#5762),#833,.T.);
#18207=ADVANCED_FACE('',(#5763),#834,.T.);
#18208=ADVANCED_FACE('',(#5764),#835,.T.);
#18209=ADVANCED_FACE('',(#5765,#1055),#836,.T.);
#18210=ADVANCED_FACE('',(#5766),#837,.T.);
#18211=ADVANCED_FACE('',(#5767),#838,.T.);
#18212=ADVANCED_FACE('',(#5768),#839,.T.);
#18213=ADVANCED_FACE('',(#5769,#1056),#840,.T.);
#18214=ADVANCED_FACE('',(#5770),#841,.T.);
#18215=ADVANCED_FACE('',(#5771),#842,.T.);
#18216=ADVANCED_FACE('',(#5772),#843,.T.);
#18217=ADVANCED_FACE('',(#5773),#844,.T.);
#18218=ADVANCED_FACE('',(#5774,#1057),#845,.T.);
#18219=ADVANCED_FACE('',(#5775),#846,.T.);
#18220=ADVANCED_FACE('',(#5776),#847,.T.);
#18221=ADVANCED_FACE('',(#5777,#1058,#1059),#848,.F.);
#18222=ADVANCED_FACE('',(#5778),#849,.T.);
#18223=ADVANCED_FACE('',(#5779),#850,.F.);
#18224=ADVANCED_FACE('',(#5780),#851,.T.);
#18225=ADVANCED_FACE('',(#5781),#852,.T.);
#18226=ADVANCED_FACE('',(#5782),#853,.T.);
#18227=ADVANCED_FACE('',(#5783),#854,.T.);
#18228=ADVANCED_FACE('',(#5784),#855,.T.);
#18229=ADVANCED_FACE('',(#5785),#856,.T.);
#18230=ADVANCED_FACE('',(#5786),#857,.T.);
#18231=ADVANCED_FACE('',(#5787),#858,.F.);
#18232=ADVANCED_FACE('',(#5788),#859,.T.);
#18233=ADVANCED_FACE('',(#5789,#1060,#1061,#1062,#1063),#860,.T.);
#18234=ADVANCED_FACE('',(#5790),#17261,.F.);
#18235=ADVANCED_FACE('',(#5791),#4820,.T.);
#18236=ADVANCED_FACE('',(#5792),#176,.T.);
#18237=ADVANCED_FACE('',(#5793),#4821,.T.);
#18238=ADVANCED_FACE('',(#5794,#1064),#861,.T.);
#18239=ADVANCED_FACE('',(#5795),#862,.F.);
#18240=ADVANCED_FACE('',(#5796),#863,.T.);
#18241=ADVANCED_FACE('',(#5797),#864,.T.);
#18242=ADVANCED_FACE('',(#5798),#865,.T.);
#18243=ADVANCED_FACE('',(#5799),#866,.T.);
#18244=ADVANCED_FACE('',(#5800),#867,.T.);
#18245=ADVANCED_FACE('',(#5801),#868,.T.);
#18246=ADVANCED_FACE('',(#5802),#869,.F.);
#18247=ADVANCED_FACE('',(#5803),#177,.T.);
#18248=ADVANCED_FACE('',(#5804),#178,.T.);
#18249=ADVANCED_FACE('',(#5805),#179,.T.);
#18250=ADVANCED_FACE('',(#5806),#180,.T.);
#18251=ADVANCED_FACE('',(#5807),#181,.T.);
#18252=ADVANCED_FACE('',(#5808),#182,.T.);
#18253=ADVANCED_FACE('',(#5809),#870,.F.);
#18254=ADVANCED_FACE('',(#5810),#871,.F.);
#18255=ADVANCED_FACE('',(#5811),#872,.F.);
#18256=ADVANCED_FACE('',(#5812),#873,.F.);
#18257=ADVANCED_FACE('',(#5813),#874,.F.);
#18258=ADVANCED_FACE('',(#5814),#875,.F.);
#18259=CLOSED_SHELL('',(#17262,#17263,#17264,#17265,#17266,#17267,#17268,
#17269,#17270,#17271,#17272,#17273,#17274,#17275,#17276,#17277,#17278,#17279,
#17280,#17281,#17282,#17283,#17284,#17285,#17286,#17287,#17288,#17289,#17290,
#17291,#17292,#17293,#17294,#17295,#17296,#17297,#17298,#17299,#17300,#17301,
#17302,#17303,#17304,#17305,#17306,#17307,#17308,#17309,#17310,#17311,#17312,
#17313,#17314,#17315,#17316,#17317,#17318,#17319,#17320,#17321,#17322,#17323,
#17324,#17325,#17326,#17327,#17328,#17329,#17330,#17331,#17332,#17333,#17334,
#17335,#17336,#17337,#17338,#17339,#17340,#17341,#17342,#17343,#17344,#17345,
#17346,#17347));
#18260=CLOSED_SHELL('',(#17348,#17349,#17350,#17351,#17352,#17353,#17354,
#17355,#17356,#17357,#17358,#17359,#17360,#17361,#17362,#17363,#17364,#17365,
#17366,#17367,#17368,#17369,#17370,#17371,#17372,#17373,#17374,#17375,#17376,
#17377,#17378,#17379,#17380,#17381,#17382,#17383,#17384,#17385,#17386,#17387,
#17388,#17389,#17390,#17391,#17392,#17393,#17394,#17395,#17396,#17397,#17398,
#17399,#17400,#17401,#17402,#17403,#17404,#17405,#17406,#17407,#17408,#17409,
#17410,#17411,#17412,#17413,#17414,#17415,#17416,#17417,#17418,#17419,#17420,
#17421,#17422,#17423,#17424,#17425,#17426,#17427,#17428,#17429,#17430,#17431,
#17432,#17433,#17434,#17435,#17436,#17437,#17438,#17439,#17440,#17441,#17442,
#17443,#17444,#17445,#17446,#17447,#17448,#17449,#17450,#17451));
#18261=CLOSED_SHELL('',(#17452,#17453,#17454,#17455,#17456,#17457,#17458,
#17459,#17460,#17461,#17462,#17463,#17464,#17465));
#18262=CLOSED_SHELL('',(#17466,#17467,#17468,#17469,#17470,#17471,#17472,
#17473,#17474,#17475,#17476,#17477,#17478,#17479,#17480,#17481,#17482,#17483,
#17484,#17485,#17486,#17487,#17488,#17489,#17490,#17491,#17492,#17493,#17494,
#17495,#17496,#17497));
#18263=CLOSED_SHELL('',(#17498,#17499,#17500,#17501,#17502,#17503,#17504,
#17505,#17506,#17507,#17508,#17509,#17510,#17511,#17512,#17513,#17514,#17515,
#17516));
#18264=CLOSED_SHELL('',(#17517,#17518,#17519));
#18265=CLOSED_SHELL('',(#17520,#17521,#17522,#17523,#17524,#17525,#17526,
#17527,#17528,#17529,#17530));
#18266=CLOSED_SHELL('',(#17531,#17532,#17533));
#18267=CLOSED_SHELL('',(#17534,#17535));
#18268=CLOSED_SHELL('',(#17536,#17537,#17538,#17539,#17540,#17541,#17542,
#17543,#17544));
#18269=CLOSED_SHELL('',(#17545,#17546,#17547,#17548,#17549,#17550,#17551,
#17552,#17553,#17554,#17555,#17556,#17557,#17558,#17559,#17560,#17561,#17562,
#17563,#17564,#17565,#17566,#17567,#17568,#17569,#17570,#17571,#17572,#17573,
#17574,#17575,#17576,#17577,#17578,#17579,#17580,#17581,#17582,#17583,#17584,
#17585,#17586,#17587,#17588,#17589,#17590,#17591,#17592,#17593,#17594,#17595,
#17596,#17597,#17598,#17599,#17600,#17601,#17602,#17603,#17604,#17605,#17606,
#17607,#17608,#17609,#17610,#17611,#17612,#17613,#17614,#17615,#17616,#17617,
#17618,#17619,#17620,#17621,#17622,#17623,#17624,#17625,#17626,#17627,#17628,
#17629,#17630,#17631,#17632,#17633,#17634,#17635,#17636,#17637,#17638,#17639,
#17640,#17641,#17642,#17643,#17644,#17645,#17646,#17647,#17648,#17649,#17650,
#17651,#17652,#17653,#17654,#17655,#17656,#17657,#17658,#17659,#17660,#17661,
#17662,#17663,#17664,#17665,#17666,#17667,#17668,#17669,#17670,#17671,#17672,
#17673,#17674,#17675,#17676,#17677,#17678,#17679,#17680,#17681,#17682,#17683,
#17684,#17685,#17686,#17687,#17688,#17689,#17690,#17691,#17692,#17693,#17694,
#17695,#17696,#17697,#17698,#17699,#17700,#17701,#17702,#17703,#17704,#17705,
#17706,#17707,#17708,#17709,#17710,#17711,#17712,#17713,#17714,#17715,#17716,
#17717,#17718,#17719,#17720,#17721,#17722,#17723,#17724,#17725,#17726,#17727,
#17728,#17729,#17730,#17731,#17732,#17733,#17734,#17735,#17736,#17737,#17738,
#17739,#17740,#17741,#17742,#17743,#17744,#17745,#17746,#17747,#17748,#17749,
#17750,#17751,#17752,#17753,#17754,#17755,#17756,#17757,#17758,#17759,#17760,
#17761,#17762,#17763,#17764,#17765,#17766,#17767,#17768,#17769,#17770,#17771,
#17772,#17773,#17774,#17775,#17776,#17777,#17778,#17779,#17780,#17781,#17782,
#17783,#17784,#17785,#17786,#17787,#17788,#17789,#17790,#17791,#17792,#17793,
#17794,#17795,#17796,#17797,#17798,#17799,#17800,#17801,#17802,#17803,#17804,
#17805,#17806,#17807,#17808,#17809,#17810,#17811,#17812,#17813,#17814,#17815,
#17816,#17817,#17818,#17819,#17820,#17821,#17822,#17823,#17824,#17825,#17826,
#17827,#17828,#17829,#17830,#17831,#17832,#17833,#17834,#17835,#17836,#17837,
#17838,#17839,#17840,#17841,#17842,#17843,#17844,#17845,#17846,#17847,#17848,
#17849,#17850,#17851,#17852,#17853,#17854,#17855,#17856,#17857,#17858,#17859,
#17860,#17861,#17862,#17863,#17864,#17865,#17866,#17867,#17868,#17869,#17870,
#17871,#17872,#17873,#17874,#17875,#17876,#17877,#17878,#17879,#17880,#17881,
#17882,#17883,#17884,#17885,#17886,#17887,#17888,#17889,#17890,#17891,#17892,
#17893,#17894,#17895,#17896,#17897,#17898,#17899,#17900,#17901,#17902,#17903,
#17904,#17905,#17906,#17907,#17908,#17909,#17910,#17911,#17912,#17913,#17914,
#17915,#17916,#17917,#17918,#17919,#17920,#17921,#17922,#17923,#17924,#17925,
#17926,#17927,#17928,#17929,#17930,#17931,#17932,#17933,#17934,#17935,#17936,
#17937,#17938,#17939,#17940,#17941,#17942,#17943,#17944,#17945,#17946,#17947,
#17948,#17949,#17950,#17951,#17952,#17953,#17954,#17955,#17956,#17957,#17958,
#17959,#17960,#17961,#17962,#17963,#17964,#17965,#17966,#17967,#17968,#17969,
#17970,#17971,#17972,#17973,#17974,#17975,#17976,#17977,#17978,#17979,#17980,
#17981,#17982,#17983,#17984,#17985,#17986,#17987,#17988,#17989,#17990,#17991,
#17992,#17993,#17994,#17995,#17996,#17997,#17998,#17999,#18000,#18001,#18002,
#18003,#18004,#18005,#18006,#18007,#18008,#18009,#18010,#18011,#18012,#18013,
#18014,#18015,#18016,#18017,#18018,#18019,#18020,#18021,#18022,#18023,#18024,
#18025,#18026,#18027,#18028,#18029,#18030,#18031,#18032,#18033,#18034,#18035,
#18036,#18037,#18038,#18039,#18040,#18041,#18042,#18043,#18044,#18045,#18046,
#18047,#18048,#18049,#18050,#18051,#18052,#18053,#18054,#18055,#18056,#18057,
#18058,#18059,#18060,#18061,#18062,#18063,#18064,#18065,#18066,#18067,#18068,
#18069,#18070,#18071,#18072,#18073,#18074,#18075,#18076,#18077,#18078,#18079,
#18080,#18081,#18082,#18083,#18084,#18085,#18086,#18087,#18088,#18089,#18090,
#18091,#18092,#18093,#18094,#18095,#18096,#18097,#18098,#18099,#18100,#18101,
#18102,#18103,#18104,#18105,#18106,#18107,#18108,#18109,#18110,#18111,#18112,
#18113,#18114,#18115,#18116,#18117,#18118,#18119,#18120,#18121,#18122,#18123,
#18124,#18125,#18126,#18127,#18128,#18129,#18130,#18131,#18132,#18133,#18134,
#18135,#18136,#18137,#18138,#18139,#18140,#18141,#18142,#18143,#18144,#18145,
#18146,#18147,#18148,#18149,#18150,#18151,#18152,#18153,#18154,#18155,#18156,
#18157,#18158,#18159,#18160,#18161,#18162,#18163,#18164,#18165,#18166,#18167,
#18168,#18169,#18170,#18171,#18172,#18173,#18174,#18175,#18176,#18177,#18178,
#18179,#18180,#18181,#18182,#18183,#18184,#18185,#18186,#18187,#18188,#18189,
#18190,#18191,#18192,#18193,#18194,#18195,#18196,#18197,#18198,#18199,#18200,
#18201,#18202,#18203,#18204,#18205,#18206,#18207,#18208,#18209,#18210,#18211,
#18212,#18213,#18214,#18215,#18216,#18217,#18218,#18219,#18220,#18221,#18222,
#18223,#18224,#18225,#18226,#18227,#18228,#18229,#18230,#18231,#18232,#18233));
#18270=CLOSED_SHELL('',(#18234,#18235,#18236,#18237,#18238,#18239,#18240,
#18241,#18242,#18243,#18244,#18245,#18246,#18247,#18248,#18249,#18250,#18251,
#18252,#18253,#18254,#18255,#18256,#18257,#18258));
#18271=DERIVED_UNIT_ELEMENT(#18285,1.);
#18272=DERIVED_UNIT_ELEMENT(#39961,-3.);
#18273=DERIVED_UNIT_ELEMENT(#18285,1.);
#18274=DERIVED_UNIT_ELEMENT(#39961,-3.);
#18275=DERIVED_UNIT_ELEMENT(#18285,1.);
#18276=DERIVED_UNIT_ELEMENT(#39961,-3.);
#18277=DERIVED_UNIT_ELEMENT(#18285,1.);
#18278=DERIVED_UNIT_ELEMENT(#39961,-3.);
#18279=DERIVED_UNIT_ELEMENT(#18285,1.);
#18280=DERIVED_UNIT_ELEMENT(#39961,-3.);
#18281=DERIVED_UNIT_ELEMENT(#18285,1.);
#18282=DERIVED_UNIT_ELEMENT(#39961,-3.);
#18283=DERIVED_UNIT_ELEMENT(#18285,1.);
#18284=DERIVED_UNIT_ELEMENT(#39961,-3.);
#18285=(
MASS_UNIT()
NAMED_UNIT(*)
SI_UNIT(.KILO.,.GRAM.)
);
#18286=DERIVED_UNIT((#18271,#18272));
#18287=DERIVED_UNIT((#18273,#18274));
#18288=DERIVED_UNIT((#18275,#18276));
#18289=DERIVED_UNIT((#18277,#18278));
#18290=DERIVED_UNIT((#18279,#18280));
#18291=DERIVED_UNIT((#18281,#18282));
#18292=DERIVED_UNIT((#18283,#18284));
#18293=MEASURE_REPRESENTATION_ITEM('density measure',
POSITIVE_RATIO_MEASURE(7850.),#18286);
#18294=MEASURE_REPRESENTATION_ITEM('density measure',
POSITIVE_RATIO_MEASURE(7850.),#18287);
#18295=MEASURE_REPRESENTATION_ITEM('density measure',
POSITIVE_RATIO_MEASURE(7850.),#18288);
#18296=MEASURE_REPRESENTATION_ITEM('density measure',
POSITIVE_RATIO_MEASURE(7850.),#18289);
#18297=MEASURE_REPRESENTATION_ITEM('density measure',
POSITIVE_RATIO_MEASURE(7850.),#18290);
#18298=MEASURE_REPRESENTATION_ITEM('density measure',
POSITIVE_RATIO_MEASURE(7850.),#18291);
#18299=MEASURE_REPRESENTATION_ITEM('density measure',
POSITIVE_RATIO_MEASURE(7850.),#18292);
#18300=PROPERTY_DEFINITION_REPRESENTATION(#18335,#18314);
#18301=PROPERTY_DEFINITION_REPRESENTATION(#18336,#18315);
#18302=PROPERTY_DEFINITION_REPRESENTATION(#18337,#18316);
#18303=PROPERTY_DEFINITION_REPRESENTATION(#18338,#18317);
#18304=PROPERTY_DEFINITION_REPRESENTATION(#18339,#18318);
#18305=PROPERTY_DEFINITION_REPRESENTATION(#18340,#18319);
#18306=PROPERTY_DEFINITION_REPRESENTATION(#18341,#18320);
#18307=PROPERTY_DEFINITION_REPRESENTATION(#18342,#18321);
#18308=PROPERTY_DEFINITION_REPRESENTATION(#18343,#18322);
#18309=PROPERTY_DEFINITION_REPRESENTATION(#18344,#18323);
#18310=PROPERTY_DEFINITION_REPRESENTATION(#18345,#18324);
#18311=PROPERTY_DEFINITION_REPRESENTATION(#18346,#18325);
#18312=PROPERTY_DEFINITION_REPRESENTATION(#18347,#18326);
#18313=PROPERTY_DEFINITION_REPRESENTATION(#18348,#18327);
#18314=REPRESENTATION('material name',(#18328),#39952);
#18315=REPRESENTATION('density',(#18293),#39952);
#18316=REPRESENTATION('material name',(#18329),#39953);
#18317=REPRESENTATION('density',(#18294),#39953);
#18318=REPRESENTATION('material name',(#18330),#39954);
#18319=REPRESENTATION('density',(#18295),#39954);
#18320=REPRESENTATION('material name',(#18331),#39955);
#18321=REPRESENTATION('density',(#18296),#39955);
#18322=REPRESENTATION('material name',(#18332),#39956);
#18323=REPRESENTATION('density',(#18297),#39956);
#18324=REPRESENTATION('material name',(#18333),#39957);
#18325=REPRESENTATION('density',(#18298),#39957);
#18326=REPRESENTATION('material name',(#18334),#39958);
#18327=REPRESENTATION('density',(#18299),#39958);
#18328=DESCRIPTIVE_REPRESENTATION_ITEM('Steel','Steel');
#18329=DESCRIPTIVE_REPRESENTATION_ITEM('Steel','Steel');
#18330=DESCRIPTIVE_REPRESENTATION_ITEM('Steel','Steel');
#18331=DESCRIPTIVE_REPRESENTATION_ITEM('Steel','Steel');
#18332=DESCRIPTIVE_REPRESENTATION_ITEM('Steel','Steel');
#18333=DESCRIPTIVE_REPRESENTATION_ITEM('Steel','Steel');
#18334=DESCRIPTIVE_REPRESENTATION_ITEM('Steel','Steel');
#18335=PROPERTY_DEFINITION('material property','material name',#40011);
#18336=PROPERTY_DEFINITION('material property','density of part',#40011);
#18337=PROPERTY_DEFINITION('material property','material name',#40012);
#18338=PROPERTY_DEFINITION('material property','density of part',#40012);
#18339=PROPERTY_DEFINITION('material property','material name',#40013);
#18340=PROPERTY_DEFINITION('material property','density of part',#40013);
#18341=PROPERTY_DEFINITION('material property','material name',#40014);
#18342=PROPERTY_DEFINITION('material property','density of part',#40014);
#18343=PROPERTY_DEFINITION('material property','material name',#40015);
#18344=PROPERTY_DEFINITION('material property','density of part',#40015);
#18345=PROPERTY_DEFINITION('material property','material name',#40016);
#18346=PROPERTY_DEFINITION('material property','density of part',#40016);
#18347=PROPERTY_DEFINITION('material property','material name',#40017);
#18348=PROPERTY_DEFINITION('material property','density of part',#40017);
#18349=AXIS2_PLACEMENT_3D('',#24905,#20010,#20011);
#18350=AXIS2_PLACEMENT_3D('',#24906,#20012,#20013);
#18351=AXIS2_PLACEMENT_3D('',#24907,#20014,#20015);
#18352=AXIS2_PLACEMENT_3D('',#24909,#20016,#20017);
#18353=AXIS2_PLACEMENT_3D('',#24911,#20018,#20019);
#18354=AXIS2_PLACEMENT_3D('',#24912,#20020,#20021);
#18355=AXIS2_PLACEMENT_3D('',#24913,#20022,#20023);
#18356=AXIS2_PLACEMENT_3D('',#24916,#20024,#20025);
#18357=AXIS2_PLACEMENT_3D('',#24917,#20026,#20027);
#18358=AXIS2_PLACEMENT_3D('',#24919,#20028,#20029);
#18359=AXIS2_PLACEMENT_3D('',#24920,#20030,#20031);
#18360=AXIS2_PLACEMENT_3D('',#24921,#20032,#20033);
#18361=AXIS2_PLACEMENT_3D('',#24924,#20034,#20035);
#18362=AXIS2_PLACEMENT_3D('',#24928,#20037,#20038);
#18363=AXIS2_PLACEMENT_3D('',#24932,#20040,#20041);
#18364=AXIS2_PLACEMENT_3D('',#24936,#20043,#20044);
#18365=AXIS2_PLACEMENT_3D('',#24940,#20046,#20047);
#18366=AXIS2_PLACEMENT_3D('',#24944,#20049,#20050);
#18367=AXIS2_PLACEMENT_3D('',#24948,#20052,#20053);
#18368=AXIS2_PLACEMENT_3D('',#24952,#20055,#20056);
#18369=AXIS2_PLACEMENT_3D('',#24956,#20058,#20059);
#18370=AXIS2_PLACEMENT_3D('',#24959,#20061,#20062);
#18371=AXIS2_PLACEMENT_3D('',#24961,#20063,#20064);
#18372=AXIS2_PLACEMENT_3D('',#24965,#20066,#20067);
#18373=AXIS2_PLACEMENT_3D('',#24969,#20069,#20070);
#18374=AXIS2_PLACEMENT_3D('',#24973,#20072,#20073);
#18375=AXIS2_PLACEMENT_3D('',#24977,#20075,#20076);
#18376=AXIS2_PLACEMENT_3D('',#24981,#20078,#20079);
#18377=AXIS2_PLACEMENT_3D('',#24985,#20081,#20082);
#18378=AXIS2_PLACEMENT_3D('',#24989,#20084,#20085);
#18379=AXIS2_PLACEMENT_3D('',#24993,#20087,#20088);
#18380=AXIS2_PLACEMENT_3D('',#24997,#20090,#20091);
#18381=AXIS2_PLACEMENT_3D('',#24999,#20093,#20094);
#18382=AXIS2_PLACEMENT_3D('',#25001,#20095,#20096);
#18383=AXIS2_PLACEMENT_3D('',#25004,#20098,#20099);
#18384=AXIS2_PLACEMENT_3D('',#25005,#20100,#20101);
#18385=AXIS2_PLACEMENT_3D('',#25007,#20102,#20103);
#18386=AXIS2_PLACEMENT_3D('',#25010,#20105,#20106);
#18387=AXIS2_PLACEMENT_3D('',#25011,#20107,#20108);
#18388=AXIS2_PLACEMENT_3D('',#25013,#20109,#20110);
#18389=AXIS2_PLACEMENT_3D('',#25016,#20112,#20113);
#18390=AXIS2_PLACEMENT_3D('',#25017,#20114,#20115);
#18391=AXIS2_PLACEMENT_3D('',#25019,#20116,#20117);
#18392=AXIS2_PLACEMENT_3D('',#25022,#20119,#20120);
#18393=AXIS2_PLACEMENT_3D('',#25023,#20121,#20122);
#18394=AXIS2_PLACEMENT_3D('',#25025,#20123,#20124);
#18395=AXIS2_PLACEMENT_3D('',#25028,#20126,#20127);
#18396=AXIS2_PLACEMENT_3D('',#25029,#20128,#20129);
#18397=AXIS2_PLACEMENT_3D('',#25031,#20130,#20131);
#18398=AXIS2_PLACEMENT_3D('',#25034,#20133,#20134);
#18399=AXIS2_PLACEMENT_3D('',#25035,#20135,#20136);
#18400=AXIS2_PLACEMENT_3D('',#25037,#20137,#20138);
#18401=AXIS2_PLACEMENT_3D('',#25040,#20140,#20141);
#18402=AXIS2_PLACEMENT_3D('',#25041,#20142,#20143);
#18403=AXIS2_PLACEMENT_3D('',#25043,#20144,#20145);
#18404=AXIS2_PLACEMENT_3D('',#25046,#20147,#20148);
#18405=AXIS2_PLACEMENT_3D('',#25047,#20149,#20150);
#18406=AXIS2_PLACEMENT_3D('',#25113,#20152,#20153);
#18407=AXIS2_PLACEMENT_3D('',#25114,#20154,#20155);
#18408=AXIS2_PLACEMENT_3D('',#25180,#20157,#20158);
#18409=AXIS2_PLACEMENT_3D('',#25181,#20159,#20160);
#18410=AXIS2_PLACEMENT_3D('',#25251,#20162,#20163);
#18411=AXIS2_PLACEMENT_3D('',#25252,#20164,#20165);
#18412=AXIS2_PLACEMENT_3D('',#25322,#20167,#20168);
#18413=AXIS2_PLACEMENT_3D('',#25323,#20169,#20170);
#18414=AXIS2_PLACEMENT_3D('',#25326,#20172,#20173);
#18415=AXIS2_PLACEMENT_3D('',#25327,#20174,#20175);
#18416=AXIS2_PLACEMENT_3D('',#25329,#20176,#20177);
#18417=AXIS2_PLACEMENT_3D('',#25332,#20179,#20180);
#18418=AXIS2_PLACEMENT_3D('',#25333,#20181,#20182);
#18419=AXIS2_PLACEMENT_3D('',#25335,#20183,#20184);
#18420=AXIS2_PLACEMENT_3D('',#25338,#20186,#20187);
#18421=AXIS2_PLACEMENT_3D('',#25339,#20188,#20189);
#18422=AXIS2_PLACEMENT_3D('',#25341,#20190,#20191);
#18423=AXIS2_PLACEMENT_3D('',#25344,#20193,#20194);
#18424=AXIS2_PLACEMENT_3D('',#25345,#20195,#20196);
#18425=AXIS2_PLACEMENT_3D('',#25347,#20197,#20198);
#18426=AXIS2_PLACEMENT_3D('',#25350,#20200,#20201);
#18427=AXIS2_PLACEMENT_3D('',#25351,#20202,#20203);
#18428=AXIS2_PLACEMENT_3D('',#25353,#20204,#20205);
#18429=AXIS2_PLACEMENT_3D('',#25356,#20207,#20208);
#18430=AXIS2_PLACEMENT_3D('',#25357,#20209,#20210);
#18431=AXIS2_PLACEMENT_3D('',#25359,#20211,#20212);
#18432=AXIS2_PLACEMENT_3D('',#25362,#20214,#20215);
#18433=AXIS2_PLACEMENT_3D('',#25363,#20216,#20217);
#18434=AXIS2_PLACEMENT_3D('',#25365,#20218,#20219);
#18435=AXIS2_PLACEMENT_3D('',#25368,#20221,#20222);
#18436=AXIS2_PLACEMENT_3D('',#25369,#20223,#20224);
#18437=AXIS2_PLACEMENT_3D('',#25371,#20225,#20226);
#18438=AXIS2_PLACEMENT_3D('',#25374,#20228,#20229);
#18439=AXIS2_PLACEMENT_3D('',#25375,#20230,#20231);
#18440=AXIS2_PLACEMENT_3D('',#25377,#20232,#20233);
#18441=AXIS2_PLACEMENT_3D('',#25380,#20235,#20236);
#18442=AXIS2_PLACEMENT_3D('',#25381,#20237,#20238);
#18443=AXIS2_PLACEMENT_3D('',#25383,#20239,#20240);
#18444=AXIS2_PLACEMENT_3D('',#25386,#20242,#20243);
#18445=AXIS2_PLACEMENT_3D('',#25387,#20244,#20245);
#18446=AXIS2_PLACEMENT_3D('',#25389,#20246,#20247);
#18447=AXIS2_PLACEMENT_3D('',#25392,#20249,#20250);
#18448=AXIS2_PLACEMENT_3D('',#25393,#20251,#20252);
#18449=AXIS2_PLACEMENT_3D('',#25395,#20253,#20254);
#18450=AXIS2_PLACEMENT_3D('',#25398,#20256,#20257);
#18451=AXIS2_PLACEMENT_3D('',#25399,#20258,#20259);
#18452=AXIS2_PLACEMENT_3D('',#25401,#20260,#20261);
#18453=AXIS2_PLACEMENT_3D('',#25404,#20263,#20264);
#18454=AXIS2_PLACEMENT_3D('',#25405,#20265,#20266);
#18455=AXIS2_PLACEMENT_3D('',#25407,#20267,#20268);
#18456=AXIS2_PLACEMENT_3D('',#25410,#20270,#20271);
#18457=AXIS2_PLACEMENT_3D('',#25411,#20272,#20273);
#18458=AXIS2_PLACEMENT_3D('',#25413,#20274,#20275);
#18459=AXIS2_PLACEMENT_3D('',#25416,#20277,#20278);
#18460=AXIS2_PLACEMENT_3D('',#25417,#20279,#20280);
#18461=AXIS2_PLACEMENT_3D('',#25420,#20282,#20283);
#18462=AXIS2_PLACEMENT_3D('',#25421,#20284,#20285);
#18463=AXIS2_PLACEMENT_3D('',#25423,#20286,#20287);
#18464=AXIS2_PLACEMENT_3D('',#25426,#20289,#20290);
#18465=AXIS2_PLACEMENT_3D('',#25427,#20291,#20292);
#18466=AXIS2_PLACEMENT_3D('',#25429,#20293,#20294);
#18467=AXIS2_PLACEMENT_3D('',#25432,#20296,#20297);
#18468=AXIS2_PLACEMENT_3D('',#25433,#20298,#20299);
#18469=AXIS2_PLACEMENT_3D('',#25479,#20327,#20328);
#18470=AXIS2_PLACEMENT_3D('',#25480,#20329,#20330);
#18471=AXIS2_PLACEMENT_3D('',#25481,#20331,#20332);
#18472=AXIS2_PLACEMENT_3D('',#25482,#20333,#20334);
#18473=AXIS2_PLACEMENT_3D('',#25485,#20335,#20336);
#18474=AXIS2_PLACEMENT_3D('',#25489,#20338,#20339);
#18475=AXIS2_PLACEMENT_3D('',#25493,#20341,#20342);
#18476=AXIS2_PLACEMENT_3D('',#25497,#20344,#20345);
#18477=AXIS2_PLACEMENT_3D('',#25499,#20347,#20348);
#18478=AXIS2_PLACEMENT_3D('',#25502,#20349,#20350);
#18479=AXIS2_PLACEMENT_3D('',#25506,#20352,#20353);
#18480=AXIS2_PLACEMENT_3D('',#25510,#20355,#20356);
#18481=AXIS2_PLACEMENT_3D('',#25514,#20358,#20359);
#18482=AXIS2_PLACEMENT_3D('',#25516,#20361,#20362);
#18483=AXIS2_PLACEMENT_3D('',#25519,#20365,#20366);
#18484=AXIS2_PLACEMENT_3D('',#25521,#20368,#20369);
#18485=AXIS2_PLACEMENT_3D('',#25523,#20371,#20372);
#18486=AXIS2_PLACEMENT_3D('',#25525,#20374,#20375);
#18487=AXIS2_PLACEMENT_3D('',#25527,#20377,#20378);
#18488=AXIS2_PLACEMENT_3D('',#25529,#20380,#20381);
#18489=AXIS2_PLACEMENT_3D('',#25531,#20383,#20384);
#18490=AXIS2_PLACEMENT_3D('',#25532,#20385,#20386);
#18491=AXIS2_PLACEMENT_3D('',#25535,#20387,#20388);
#18492=AXIS2_PLACEMENT_3D('',#25539,#20390,#20391);
#18493=AXIS2_PLACEMENT_3D('',#25543,#20393,#20394);
#18494=AXIS2_PLACEMENT_3D('',#25547,#20396,#20397);
#18495=AXIS2_PLACEMENT_3D('',#25549,#20399,#20400);
#18496=AXIS2_PLACEMENT_3D('',#25552,#20401,#20402);
#18497=AXIS2_PLACEMENT_3D('',#25556,#20404,#20405);
#18498=AXIS2_PLACEMENT_3D('',#25560,#20407,#20408);
#18499=AXIS2_PLACEMENT_3D('',#25564,#20410,#20411);
#18500=AXIS2_PLACEMENT_3D('',#25566,#20413,#20414);
#18501=AXIS2_PLACEMENT_3D('',#25569,#20417,#20418);
#18502=AXIS2_PLACEMENT_3D('',#25571,#20420,#20421);
#18503=AXIS2_PLACEMENT_3D('',#25573,#20423,#20424);
#18504=AXIS2_PLACEMENT_3D('',#25575,#20426,#20427);
#18505=AXIS2_PLACEMENT_3D('',#25577,#20429,#20430);
#18506=AXIS2_PLACEMENT_3D('',#25579,#20432,#20433);
#18507=AXIS2_PLACEMENT_3D('',#25581,#20435,#20436);
#18508=AXIS2_PLACEMENT_3D('',#25582,#20437,#20438);
#18509=AXIS2_PLACEMENT_3D('',#25583,#20439,#20440);
#18510=AXIS2_PLACEMENT_3D('',#25585,#20442,#20443);
#18511=AXIS2_PLACEMENT_3D('',#25587,#20445,#20446);
#18512=AXIS2_PLACEMENT_3D('',#25588,#20447,#20448);
#18513=AXIS2_PLACEMENT_3D('',#25590,#20450,#20451);
#18514=AXIS2_PLACEMENT_3D('',#25592,#20453,#20454);
#18515=AXIS2_PLACEMENT_3D('',#25593,#20455,#20456);
#18516=AXIS2_PLACEMENT_3D('',#25595,#20458,#20459);
#18517=AXIS2_PLACEMENT_3D('',#25597,#20461,#20462);
#18518=AXIS2_PLACEMENT_3D('',#25598,#20463,#20464);
#18519=AXIS2_PLACEMENT_3D('',#25600,#20466,#20467);
#18520=AXIS2_PLACEMENT_3D('',#25602,#20469,#20470);
#18521=AXIS2_PLACEMENT_3D('',#25603,#20471,#20472);
#18522=AXIS2_PLACEMENT_3D('',#25605,#20474,#20475);
#18523=AXIS2_PLACEMENT_3D('',#25607,#20477,#20478);
#18524=AXIS2_PLACEMENT_3D('',#25608,#20479,#20480);
#18525=AXIS2_PLACEMENT_3D('',#25610,#20482,#20483);
#18526=AXIS2_PLACEMENT_3D('',#25612,#20485,#20486);
#18527=AXIS2_PLACEMENT_3D('',#25613,#20487,#20488);
#18528=AXIS2_PLACEMENT_3D('',#25615,#20490,#20491);
#18529=AXIS2_PLACEMENT_3D('',#25617,#20493,#20494);
#18530=AXIS2_PLACEMENT_3D('',#25618,#20495,#20496);
#18531=AXIS2_PLACEMENT_3D('',#25620,#20498,#20499);
#18532=AXIS2_PLACEMENT_3D('',#25622,#20501,#20502);
#18533=AXIS2_PLACEMENT_3D('',#25623,#20503,#20504);
#18534=AXIS2_PLACEMENT_3D('',#25625,#20506,#20507);
#18535=AXIS2_PLACEMENT_3D('',#25627,#20509,#20510);
#18536=AXIS2_PLACEMENT_3D('',#25628,#20511,#20512);
#18537=AXIS2_PLACEMENT_3D('',#25629,#20513,#20514);
#18538=AXIS2_PLACEMENT_3D('',#25632,#20515,#20516);
#18539=AXIS2_PLACEMENT_3D('',#25636,#20518,#20519);
#18540=AXIS2_PLACEMENT_3D('',#25638,#20521,#20522);
#18541=AXIS2_PLACEMENT_3D('',#25639,#20523,#20524);
#18542=AXIS2_PLACEMENT_3D('',#25640,#20525,#20526);
#18543=AXIS2_PLACEMENT_3D('',#25641,#20527,#20528);
#18544=AXIS2_PLACEMENT_3D('',#25643,#20529,#20530);
#18545=AXIS2_PLACEMENT_3D('',#25712,#20532,#20533);
#18546=AXIS2_PLACEMENT_3D('',#25715,#20534,#20535);
#18547=AXIS2_PLACEMENT_3D('',#25719,#20537,#20538);
#18548=AXIS2_PLACEMENT_3D('',#25721,#20540,#20541);
#18549=AXIS2_PLACEMENT_3D('',#25722,#20542,#20543);
#18550=AXIS2_PLACEMENT_3D('',#25723,#20544,#20545);
#18551=AXIS2_PLACEMENT_3D('',#25724,#20546,#20547);
#18552=AXIS2_PLACEMENT_3D('',#25727,#20548,#20549);
#18553=AXIS2_PLACEMENT_3D('',#25728,#20550,#20551);
#18554=AXIS2_PLACEMENT_3D('',#25729,#20552,#20553);
#18555=AXIS2_PLACEMENT_3D('',#25730,#20554,#20555);
#18556=AXIS2_PLACEMENT_3D('',#25734,#20557,#20558);
#18557=AXIS2_PLACEMENT_3D('',#25736,#20560,#20561);
#18558=AXIS2_PLACEMENT_3D('',#25737,#20562,#20563);
#18559=AXIS2_PLACEMENT_3D('',#25738,#20564,#20565);
#18560=AXIS2_PLACEMENT_3D('',#25739,#20566,#20567);
#18561=AXIS2_PLACEMENT_3D('',#25740,#20568,#20569);
#18562=AXIS2_PLACEMENT_3D('',#25799,#20570,#20571);
#18563=AXIS2_PLACEMENT_3D('',#25837,#20572,#20573);
#18564=AXIS2_PLACEMENT_3D('',#25890,#20574,#20575);
#18565=AXIS2_PLACEMENT_3D('',#25943,#20576,#20577);
#18566=AXIS2_PLACEMENT_3D('',#25990,#20578,#20579);
#18567=AXIS2_PLACEMENT_3D('',#26046,#20580,#20581);
#18568=AXIS2_PLACEMENT_3D('',#26093,#20582,#20583);
#18569=AXIS2_PLACEMENT_3D('',#26140,#20584,#20585);
#18570=AXIS2_PLACEMENT_3D('',#26143,#20586,#20587);
#18571=AXIS2_PLACEMENT_3D('',#26147,#20589,#20590);
#18572=AXIS2_PLACEMENT_3D('',#26149,#20592,#20593);
#18573=AXIS2_PLACEMENT_3D('',#26150,#20594,#20595);
#18574=AXIS2_PLACEMENT_3D('',#26151,#20596,#20597);
#18575=AXIS2_PLACEMENT_3D('',#26152,#20598,#20599);
#18576=AXIS2_PLACEMENT_3D('',#26154,#20600,#20601);
#18577=AXIS2_PLACEMENT_3D('',#26223,#20603,#20604);
#18578=AXIS2_PLACEMENT_3D('',#26226,#20605,#20606);
#18579=AXIS2_PLACEMENT_3D('',#26230,#20608,#20609);
#18580=AXIS2_PLACEMENT_3D('',#26232,#20611,#20612);
#18581=AXIS2_PLACEMENT_3D('',#26234,#20613,#20614);
#18582=AXIS2_PLACEMENT_3D('',#26235,#20615,#20616);
#18583=AXIS2_PLACEMENT_3D('',#26236,#20617,#20618);
#18584=AXIS2_PLACEMENT_3D('',#26238,#20619,#20620);
#18585=AXIS2_PLACEMENT_3D('',#26239,#20621,#20622);
#18586=AXIS2_PLACEMENT_3D('',#26242,#20623,#20624);
#18587=AXIS2_PLACEMENT_3D('',#26243,#20625,#20626);
#18588=AXIS2_PLACEMENT_3D('',#26244,#20627,#20628);
#18589=AXIS2_PLACEMENT_3D('',#26245,#20629,#20630);
#18590=AXIS2_PLACEMENT_3D('',#26249,#20632,#20633);
#18591=AXIS2_PLACEMENT_3D('',#26251,#20635,#20636);
#18592=AXIS2_PLACEMENT_3D('',#26252,#20637,#20638);
#18593=AXIS2_PLACEMENT_3D('',#26253,#20639,#20640);
#18594=AXIS2_PLACEMENT_3D('',#26254,#20641,#20642);
#18595=AXIS2_PLACEMENT_3D('',#26255,#20643,#20644);
#18596=AXIS2_PLACEMENT_3D('',#26260,#20645,#20646);
#18597=AXIS2_PLACEMENT_3D('',#26265,#20647,#20648);
#18598=AXIS2_PLACEMENT_3D('',#26270,#20649,#20650);
#18599=AXIS2_PLACEMENT_3D('',#26275,#20651,#20652);
#18600=AXIS2_PLACEMENT_3D('',#26282,#20653,#20654);
#18601=AXIS2_PLACEMENT_3D('',#26287,#20655,#20656);
#18602=AXIS2_PLACEMENT_3D('',#26292,#20657,#20658);
#18603=AXIS2_PLACEMENT_3D('',#26345,#20661,#20662);
#18604=AXIS2_PLACEMENT_3D('',#26348,#20663,#20664);
#18605=AXIS2_PLACEMENT_3D('',#26352,#20666,#20667);
#18606=AXIS2_PLACEMENT_3D('',#26354,#20669,#20670);
#18607=AXIS2_PLACEMENT_3D('',#26357,#20671,#20672);
#18608=AXIS2_PLACEMENT_3D('',#26361,#20674,#20675);
#18609=AXIS2_PLACEMENT_3D('',#26563,#20679,#20680);
#18610=AXIS2_PLACEMENT_3D('',#26566,#20681,#20682);
#18611=AXIS2_PLACEMENT_3D('',#26570,#20684,#20685);
#18612=AXIS2_PLACEMENT_3D('',#26572,#20687,#20688);
#18613=AXIS2_PLACEMENT_3D('',#26575,#20689,#20690);
#18614=AXIS2_PLACEMENT_3D('',#26579,#20692,#20693);
#18615=AXIS2_PLACEMENT_3D('',#26581,#20695,#20696);
#18616=AXIS2_PLACEMENT_3D('',#26584,#20697,#20698);
#18617=AXIS2_PLACEMENT_3D('',#26588,#20700,#20701);
#18618=AXIS2_PLACEMENT_3D('',#26590,#20703,#20704);
#18619=AXIS2_PLACEMENT_3D('',#26592,#20705,#20706);
#18620=AXIS2_PLACEMENT_3D('',#26596,#20709,#20710);
#18621=AXIS2_PLACEMENT_3D('',#26597,#20711,#20712);
#18622=AXIS2_PLACEMENT_3D('',#26599,#20713,#20714);
#18623=AXIS2_PLACEMENT_3D('',#26608,#20717,#20718);
#18624=AXIS2_PLACEMENT_3D('',#26806,#20719,#20720);
#18625=AXIS2_PLACEMENT_3D('',#26808,#20721,#20722);
#18626=AXIS2_PLACEMENT_3D('',#26813,#20725,#20726);
#18627=AXIS2_PLACEMENT_3D('',#26814,#20727,#20728);
#18628=AXIS2_PLACEMENT_3D('',#26816,#20729,#20730);
#18629=AXIS2_PLACEMENT_3D('',#26819,#20732,#20733);
#18630=AXIS2_PLACEMENT_3D('',#26821,#20734,#20735);
#18631=AXIS2_PLACEMENT_3D('',#26824,#20737,#20738);
#18632=AXIS2_PLACEMENT_3D('',#26825,#20739,#20740);
#18633=AXIS2_PLACEMENT_3D('',#26827,#20741,#20742);
#18634=AXIS2_PLACEMENT_3D('',#26829,#20743,#20744);
#18635=AXIS2_PLACEMENT_3D('',#26831,#20745,#20746);
#18636=AXIS2_PLACEMENT_3D('',#26832,#20747,#20748);
#18637=AXIS2_PLACEMENT_3D('',#26833,#20749,#20750);
#18638=AXIS2_PLACEMENT_3D('',#26835,#20751,#20752);
#18639=AXIS2_PLACEMENT_3D('',#26837,#20753,#20754);
#18640=AXIS2_PLACEMENT_3D('',#26839,#20755,#20756);
#18641=AXIS2_PLACEMENT_3D('',#26840,#20757,#20758);
#18642=AXIS2_PLACEMENT_3D('',#26847,#20761,#20762);
#18643=AXIS2_PLACEMENT_3D('',#26860,#20769,#20770);
#18644=AXIS2_PLACEMENT_3D('',#26868,#20774,#20775);
#18645=AXIS2_PLACEMENT_3D('',#26876,#20779,#20780);
#18646=AXIS2_PLACEMENT_3D('',#26886,#20785,#20786);
#18647=AXIS2_PLACEMENT_3D('',#26898,#20792,#20793);
#18648=AXIS2_PLACEMENT_3D('',#26906,#20797,#20798);
#18649=AXIS2_PLACEMENT_3D('',#26914,#20802,#20803);
#18650=AXIS2_PLACEMENT_3D('',#26916,#20805,#20806);
#18651=AXIS2_PLACEMENT_3D('',#26920,#20808,#20809);
#18652=AXIS2_PLACEMENT_3D('',#26922,#20811,#20812);
#18653=AXIS2_PLACEMENT_3D('',#26926,#20814,#20815);
#18654=AXIS2_PLACEMENT_3D('',#26928,#20817,#20818);
#18655=AXIS2_PLACEMENT_3D('',#26932,#20820,#20821);
#18656=AXIS2_PLACEMENT_3D('',#26934,#20823,#20824);
#18657=AXIS2_PLACEMENT_3D('',#26938,#20826,#20827);
#18658=AXIS2_PLACEMENT_3D('',#26940,#20829,#20830);
#18659=AXIS2_PLACEMENT_3D('',#26944,#20832,#20833);
#18660=AXIS2_PLACEMENT_3D('',#26946,#20835,#20836);
#18661=AXIS2_PLACEMENT_3D('',#26951,#20839,#20840);
#18662=AXIS2_PLACEMENT_3D('',#26952,#20841,#20842);
#18663=AXIS2_PLACEMENT_3D('',#26956,#20844,#20845);
#18664=AXIS2_PLACEMENT_3D('',#26958,#20847,#20848);
#18665=AXIS2_PLACEMENT_3D('',#26962,#20850,#20851);
#18666=AXIS2_PLACEMENT_3D('',#26964,#20853,#20854);
#18667=AXIS2_PLACEMENT_3D('',#26965,#20855,#20856);
#18668=AXIS2_PLACEMENT_3D('',#26966,#20857,#20858);
#18669=AXIS2_PLACEMENT_3D('',#26970,#20860,#20861);
#18670=AXIS2_PLACEMENT_3D('',#26972,#20863,#20864);
#18671=AXIS2_PLACEMENT_3D('',#26974,#20865,#20866);
#18672=AXIS2_PLACEMENT_3D('',#26976,#20868,#20869);
#18673=AXIS2_PLACEMENT_3D('',#26977,#20870,#20871);
#18674=AXIS2_PLACEMENT_3D('',#26978,#20872,#20873);
#18675=AXIS2_PLACEMENT_3D('',#26980,#20874,#20875);
#18676=AXIS2_PLACEMENT_3D('',#26982,#20877,#20878);
#18677=AXIS2_PLACEMENT_3D('',#26984,#20879,#20880);
#18678=AXIS2_PLACEMENT_3D('',#26986,#20882,#20883);
#18679=AXIS2_PLACEMENT_3D('',#26988,#20884,#20885);
#18680=AXIS2_PLACEMENT_3D('',#26990,#20887,#20888);
#18681=AXIS2_PLACEMENT_3D('',#26991,#20889,#20890);
#18682=AXIS2_PLACEMENT_3D('',#26992,#20891,#20892);
#18683=AXIS2_PLACEMENT_3D('',#26993,#20893,#20894);
#18684=AXIS2_PLACEMENT_3D('',#26999,#20898,#20899);
#18685=AXIS2_PLACEMENT_3D('',#27056,#20933,#20934);
#18686=AXIS2_PLACEMENT_3D('',#27057,#20935,#20936);
#18687=AXIS2_PLACEMENT_3D('',#27060,#20939,#20940);
#18688=AXIS2_PLACEMENT_3D('',#27061,#20941,#20942);
#18689=AXIS2_PLACEMENT_3D('',#27062,#20943,#20944);
#18690=AXIS2_PLACEMENT_3D('',#27065,#20947,#20948);
#18691=AXIS2_PLACEMENT_3D('',#27066,#20949,#20950);
#18692=AXIS2_PLACEMENT_3D('',#27067,#20951,#20952);
#18693=AXIS2_PLACEMENT_3D('',#27069,#20954,#20955);
#18694=AXIS2_PLACEMENT_3D('',#27071,#20957,#20958);
#18695=AXIS2_PLACEMENT_3D('',#27074,#20961,#20962);
#18696=AXIS2_PLACEMENT_3D('',#27075,#20963,#20964);
#18697=AXIS2_PLACEMENT_3D('',#27076,#20965,#20966);
#18698=AXIS2_PLACEMENT_3D('',#27078,#20968,#20969);
#18699=AXIS2_PLACEMENT_3D('',#27081,#20972,#20973);
#18700=AXIS2_PLACEMENT_3D('',#27082,#20974,#20975);
#18701=AXIS2_PLACEMENT_3D('',#27083,#20976,#20977);
#18702=AXIS2_PLACEMENT_3D('',#27086,#20980,#20981);
#18703=AXIS2_PLACEMENT_3D('',#27087,#20982,#20983);
#18704=AXIS2_PLACEMENT_3D('',#27088,#20984,#20985);
#18705=AXIS2_PLACEMENT_3D('',#27091,#20988,#20989);
#18706=AXIS2_PLACEMENT_3D('',#27092,#20990,#20991);
#18707=AXIS2_PLACEMENT_3D('',#27093,#20992,#20993);
#18708=AXIS2_PLACEMENT_3D('',#27096,#20996,#20997);
#18709=AXIS2_PLACEMENT_3D('',#27097,#20998,#20999);
#18710=AXIS2_PLACEMENT_3D('',#27098,#21000,#21001);
#18711=AXIS2_PLACEMENT_3D('',#27101,#21004,#21005);
#18712=AXIS2_PLACEMENT_3D('',#27102,#21006,#21007);
#18713=AXIS2_PLACEMENT_3D('',#27103,#21008,#21009);
#18714=AXIS2_PLACEMENT_3D('',#27106,#21012,#21013);
#18715=AXIS2_PLACEMENT_3D('',#27107,#21014,#21015);
#18716=AXIS2_PLACEMENT_3D('',#27128,#21016,#21017);
#18717=AXIS2_PLACEMENT_3D('',#27129,#21018,#21019);
#18718=AXIS2_PLACEMENT_3D('',#27154,#21020,#21021);
#18719=AXIS2_PLACEMENT_3D('',#27156,#21023,#21024);
#18720=AXIS2_PLACEMENT_3D('',#27158,#21026,#21027);
#18721=AXIS2_PLACEMENT_3D('',#27159,#21028,#21029);
#18722=AXIS2_PLACEMENT_3D('',#27160,#21030,#21031);
#18723=AXIS2_PLACEMENT_3D('',#27163,#21032,#21033);
#18724=AXIS2_PLACEMENT_3D('',#27165,#21034,#21035);
#18725=AXIS2_PLACEMENT_3D('',#27347,#21036,#21037);
#18726=AXIS2_PLACEMENT_3D('',#27349,#21038,#21039);
#18727=AXIS2_PLACEMENT_3D('',#27350,#21040,#21041);
#18728=AXIS2_PLACEMENT_3D('',#27446,#21042,#21043);
#18729=AXIS2_PLACEMENT_3D('',#27447,#21044,#21045);
#18730=AXIS2_PLACEMENT_3D('',#27450,#21046,#21047);
#18731=AXIS2_PLACEMENT_3D('',#27451,#21048,#21049);
#18732=AXIS2_PLACEMENT_3D('',#27453,#21050,#21051);
#18733=AXIS2_PLACEMENT_3D('',#27630,#21052,#21053);
#18734=AXIS2_PLACEMENT_3D('',#27632,#21054,#21055);
#18735=AXIS2_PLACEMENT_3D('',#27633,#21056,#21057);
#18736=AXIS2_PLACEMENT_3D('',#28375,#21058,#21059);
#18737=AXIS2_PLACEMENT_3D('',#28376,#21060,#21061);
#18738=AXIS2_PLACEMENT_3D('',#28377,#21062,#21063);
#18739=AXIS2_PLACEMENT_3D('',#28380,#21065,#21066);
#18740=AXIS2_PLACEMENT_3D('',#28381,#21067,#21068);
#18741=AXIS2_PLACEMENT_3D('',#28383,#21069,#21070);
#18742=AXIS2_PLACEMENT_3D('',#29072,#21072,#21073);
#18743=AXIS2_PLACEMENT_3D('',#29073,#21074,#21075);
#18744=AXIS2_PLACEMENT_3D('',#29074,#21076,#21077);
#18745=AXIS2_PLACEMENT_3D('',#29076,#21078,#21079);
#18746=AXIS2_PLACEMENT_3D('',#29078,#21081,#21082);
#18747=AXIS2_PLACEMENT_3D('',#29081,#21084,#21085);
#18748=AXIS2_PLACEMENT_3D('',#29082,#21086,#21087);
#18749=AXIS2_PLACEMENT_3D('',#29083,#21088,#21089);
#18750=AXIS2_PLACEMENT_3D('',#29084,#21090,#21091);
#18751=AXIS2_PLACEMENT_3D('',#29644,#21092,#21093);
#18752=AXIS2_PLACEMENT_3D('',#30300,#21094,#21095);
#18753=AXIS2_PLACEMENT_3D('',#30301,#21096,#21097);
#18754=AXIS2_PLACEMENT_3D('',#30303,#21098,#21099);
#18755=AXIS2_PLACEMENT_3D('',#30306,#21101,#21102);
#18756=AXIS2_PLACEMENT_3D('',#30307,#21103,#21104);
#18757=AXIS2_PLACEMENT_3D('',#30309,#21105,#21106);
#18758=AXIS2_PLACEMENT_3D('',#30312,#21108,#21109);
#18759=AXIS2_PLACEMENT_3D('',#30313,#21110,#21111);
#18760=AXIS2_PLACEMENT_3D('',#30315,#21112,#21113);
#18761=AXIS2_PLACEMENT_3D('',#30318,#21115,#21116);
#18762=AXIS2_PLACEMENT_3D('',#30319,#21117,#21118);
#18763=AXIS2_PLACEMENT_3D('',#30321,#21119,#21120);
#18764=AXIS2_PLACEMENT_3D('',#30324,#21122,#21123);
#18765=AXIS2_PLACEMENT_3D('',#30325,#21124,#21125);
#18766=AXIS2_PLACEMENT_3D('',#30350,#21138,#21139);
#18767=AXIS2_PLACEMENT_3D('',#30375,#21152,#21153);
#18768=AXIS2_PLACEMENT_3D('',#30381,#21157,#21158);
#18769=AXIS2_PLACEMENT_3D('',#30387,#21162,#21163);
#18770=AXIS2_PLACEMENT_3D('',#30393,#21167,#21168);
#18771=AXIS2_PLACEMENT_3D('',#30399,#21172,#21173);
#18772=AXIS2_PLACEMENT_3D('',#30402,#21176,#21177);
#18773=AXIS2_PLACEMENT_3D('',#30408,#21181,#21182);
#18774=AXIS2_PLACEMENT_3D('',#30414,#21186,#21187);
#18775=AXIS2_PLACEMENT_3D('',#30420,#21191,#21192);
#18776=AXIS2_PLACEMENT_3D('',#30426,#21196,#21197);
#18777=AXIS2_PLACEMENT_3D('',#30429,#21200,#21201);
#18778=AXIS2_PLACEMENT_3D('',#30430,#21202,#21203);
#18779=AXIS2_PLACEMENT_3D('',#30441,#21210,#21211);
#18780=AXIS2_PLACEMENT_3D('',#30445,#21214,#21215);
#18781=AXIS2_PLACEMENT_3D('',#30449,#21218,#21219);
#18782=AXIS2_PLACEMENT_3D('',#30458,#21225,#21226);
#18783=AXIS2_PLACEMENT_3D('',#30466,#21232,#21233);
#18784=AXIS2_PLACEMENT_3D('',#30470,#21236,#21237);
#18785=AXIS2_PLACEMENT_3D('',#30472,#21239,#21240);
#18786=AXIS2_PLACEMENT_3D('',#30473,#21241,#21242);
#18787=AXIS2_PLACEMENT_3D('',#30477,#21245,#21246);
#18788=AXIS2_PLACEMENT_3D('',#30481,#21249,#21250);
#18789=AXIS2_PLACEMENT_3D('',#30483,#21252,#21253);
#18790=AXIS2_PLACEMENT_3D('',#30485,#21255,#21256);
#18791=AXIS2_PLACEMENT_3D('',#30486,#21257,#21258);
#18792=AXIS2_PLACEMENT_3D('',#30488,#21260,#21261);
#18793=AXIS2_PLACEMENT_3D('',#30489,#21262,#21263);
#18794=AXIS2_PLACEMENT_3D('',#30490,#21264,#21265);
#18795=AXIS2_PLACEMENT_3D('',#30492,#21266,#21267);
#18796=AXIS2_PLACEMENT_3D('',#30495,#21269,#21270);
#18797=AXIS2_PLACEMENT_3D('',#30496,#21271,#21272);
#18798=AXIS2_PLACEMENT_3D('',#30498,#21273,#21274);
#18799=AXIS2_PLACEMENT_3D('',#30501,#21276,#21277);
#18800=AXIS2_PLACEMENT_3D('',#30502,#21278,#21279);
#18801=AXIS2_PLACEMENT_3D('',#30504,#21280,#21281);
#18802=AXIS2_PLACEMENT_3D('',#30507,#21283,#21284);
#18803=AXIS2_PLACEMENT_3D('',#30508,#21285,#21286);
#18804=AXIS2_PLACEMENT_3D('',#30510,#21287,#21288);
#18805=AXIS2_PLACEMENT_3D('',#30513,#21290,#21291);
#18806=AXIS2_PLACEMENT_3D('',#30514,#21292,#21293);
#18807=AXIS2_PLACEMENT_3D('',#30516,#21294,#21295);
#18808=AXIS2_PLACEMENT_3D('',#30519,#21297,#21298);
#18809=AXIS2_PLACEMENT_3D('',#30520,#21299,#21300);
#18810=AXIS2_PLACEMENT_3D('',#30522,#21301,#21302);
#18811=AXIS2_PLACEMENT_3D('',#30525,#21304,#21305);
#18812=AXIS2_PLACEMENT_3D('',#30526,#21306,#21307);
#18813=AXIS2_PLACEMENT_3D('',#30528,#21308,#21309);
#18814=AXIS2_PLACEMENT_3D('',#30531,#21311,#21312);
#18815=AXIS2_PLACEMENT_3D('',#30532,#21313,#21314);
#18816=AXIS2_PLACEMENT_3D('',#30534,#21315,#21316);
#18817=AXIS2_PLACEMENT_3D('',#30537,#21318,#21319);
#18818=AXIS2_PLACEMENT_3D('',#30538,#21320,#21321);
#18819=AXIS2_PLACEMENT_3D('',#30540,#21322,#21323);
#18820=AXIS2_PLACEMENT_3D('',#30543,#21325,#21326);
#18821=AXIS2_PLACEMENT_3D('',#30544,#21327,#21328);
#18822=AXIS2_PLACEMENT_3D('',#30546,#21329,#21330);
#18823=AXIS2_PLACEMENT_3D('',#30549,#21332,#21333);
#18824=AXIS2_PLACEMENT_3D('',#30550,#21334,#21335);
#18825=AXIS2_PLACEMENT_3D('',#30552,#21336,#21337);
#18826=AXIS2_PLACEMENT_3D('',#30555,#21339,#21340);
#18827=AXIS2_PLACEMENT_3D('',#30556,#21341,#21342);
#18828=AXIS2_PLACEMENT_3D('',#30558,#21343,#21344);
#18829=AXIS2_PLACEMENT_3D('',#30561,#21346,#21347);
#18830=AXIS2_PLACEMENT_3D('',#30562,#21348,#21349);
#18831=AXIS2_PLACEMENT_3D('',#30564,#21350,#21351);
#18832=AXIS2_PLACEMENT_3D('',#30567,#21353,#21354);
#18833=AXIS2_PLACEMENT_3D('',#30568,#21355,#21356);
#18834=AXIS2_PLACEMENT_3D('',#30570,#21357,#21358);
#18835=AXIS2_PLACEMENT_3D('',#30573,#21360,#21361);
#18836=AXIS2_PLACEMENT_3D('',#30574,#21362,#21363);
#18837=AXIS2_PLACEMENT_3D('',#30576,#21364,#21365);
#18838=AXIS2_PLACEMENT_3D('',#30579,#21367,#21368);
#18839=AXIS2_PLACEMENT_3D('',#30580,#21369,#21370);
#18840=AXIS2_PLACEMENT_3D('',#30582,#21371,#21372);
#18841=AXIS2_PLACEMENT_3D('',#30585,#21374,#21375);
#18842=AXIS2_PLACEMENT_3D('',#30586,#21376,#21377);
#18843=AXIS2_PLACEMENT_3D('',#30588,#21378,#21379);
#18844=AXIS2_PLACEMENT_3D('',#30591,#21381,#21382);
#18845=AXIS2_PLACEMENT_3D('',#30592,#21383,#21384);
#18846=AXIS2_PLACEMENT_3D('',#30593,#21385,#21386);
#18847=AXIS2_PLACEMENT_3D('',#30594,#21387,#21388);
#18848=AXIS2_PLACEMENT_3D('',#30596,#21389,#21390);
#18849=AXIS2_PLACEMENT_3D('',#30599,#21392,#21393);
#18850=AXIS2_PLACEMENT_3D('',#30600,#21394,#21395);
#18851=AXIS2_PLACEMENT_3D('',#30601,#21396,#21397);
#18852=AXIS2_PLACEMENT_3D('',#30602,#21398,#21399);
#18853=AXIS2_PLACEMENT_3D('',#30603,#21400,#21401);
#18854=AXIS2_PLACEMENT_3D('',#30605,#21402,#21403);
#18855=AXIS2_PLACEMENT_3D('',#30607,#21404,#21405);
#18856=AXIS2_PLACEMENT_3D('',#30609,#21406,#21407);
#18857=AXIS2_PLACEMENT_3D('',#30610,#21408,#21409);
#18858=AXIS2_PLACEMENT_3D('',#30611,#21410,#21411);
#18859=AXIS2_PLACEMENT_3D('',#30614,#21412,#21413);
#18860=AXIS2_PLACEMENT_3D('',#30616,#21414,#21415);
#18861=AXIS2_PLACEMENT_3D('',#30618,#21416,#21417);
#18862=AXIS2_PLACEMENT_3D('',#30619,#21418,#21419);
#18863=AXIS2_PLACEMENT_3D('',#30620,#21420,#21421);
#18864=AXIS2_PLACEMENT_3D('',#30621,#21422,#21423);
#18865=AXIS2_PLACEMENT_3D('',#30624,#21424,#21425);
#18866=AXIS2_PLACEMENT_3D('',#30626,#21426,#21427);
#18867=AXIS2_PLACEMENT_3D('',#30628,#21428,#21429);
#18868=AXIS2_PLACEMENT_3D('',#30629,#21430,#21431);
#18869=AXIS2_PLACEMENT_3D('',#30630,#21432,#21433);
#18870=AXIS2_PLACEMENT_3D('',#30631,#21434,#21435);
#18871=AXIS2_PLACEMENT_3D('',#30634,#21436,#21437);
#18872=AXIS2_PLACEMENT_3D('',#30636,#21438,#21439);
#18873=AXIS2_PLACEMENT_3D('',#30638,#21440,#21441);
#18874=AXIS2_PLACEMENT_3D('',#30639,#21442,#21443);
#18875=AXIS2_PLACEMENT_3D('',#30640,#21444,#21445);
#18876=AXIS2_PLACEMENT_3D('',#30641,#21446,#21447);
#18877=AXIS2_PLACEMENT_3D('',#30643,#21448,#21449);
#18878=AXIS2_PLACEMENT_3D('',#30646,#21451,#21452);
#18879=AXIS2_PLACEMENT_3D('',#30647,#21453,#21454);
#18880=AXIS2_PLACEMENT_3D('',#30649,#21456,#21457);
#18881=AXIS2_PLACEMENT_3D('',#30652,#21459,#21460);
#18882=AXIS2_PLACEMENT_3D('',#30653,#21461,#21462);
#18883=AXIS2_PLACEMENT_3D('',#30655,#21464,#21465);
#18884=AXIS2_PLACEMENT_3D('',#30657,#21467,#21468);
#18885=AXIS2_PLACEMENT_3D('',#30658,#21469,#21470);
#18886=AXIS2_PLACEMENT_3D('',#30659,#21471,#21472);
#18887=AXIS2_PLACEMENT_3D('',#30662,#21473,#21474);
#18888=AXIS2_PLACEMENT_3D('',#30663,#21475,#21476);
#18889=AXIS2_PLACEMENT_3D('',#30666,#21478,#21479);
#18890=AXIS2_PLACEMENT_3D('',#30667,#21480,#21481);
#18891=AXIS2_PLACEMENT_3D('',#30670,#21483,#21484);
#18892=AXIS2_PLACEMENT_3D('',#30671,#21485,#21486);
#18893=AXIS2_PLACEMENT_3D('',#30672,#21487,#21488);
#18894=AXIS2_PLACEMENT_3D('',#30676,#21490,#21491);
#18895=AXIS2_PLACEMENT_3D('',#30677,#21492,#21493);
#18896=AXIS2_PLACEMENT_3D('',#30678,#21494,#21495);
#18897=AXIS2_PLACEMENT_3D('',#30691,#21502,#21503);
#18898=AXIS2_PLACEMENT_3D('',#30697,#21507,#21508);
#18899=AXIS2_PLACEMENT_3D('',#30701,#21511,#21512);
#18900=AXIS2_PLACEMENT_3D('',#30707,#21516,#21517);
#18901=AXIS2_PLACEMENT_3D('',#30711,#21520,#21521);
#18902=AXIS2_PLACEMENT_3D('',#30715,#21524,#21525);
#18903=AXIS2_PLACEMENT_3D('',#30719,#21528,#21529);
#18904=AXIS2_PLACEMENT_3D('',#30721,#21531,#21532);
#18905=AXIS2_PLACEMENT_3D('',#30788,#21536,#21537);
#18906=AXIS2_PLACEMENT_3D('',#30790,#21538,#21539);
#18907=AXIS2_PLACEMENT_3D('',#30792,#21540,#21541);
#18908=AXIS2_PLACEMENT_3D('',#30794,#21542,#21543);
#18909=AXIS2_PLACEMENT_3D('',#30795,#21544,#21545);
#18910=AXIS2_PLACEMENT_3D('',#30796,#21546,#21547);
#18911=AXIS2_PLACEMENT_3D('',#30798,#21548,#21549);
#18912=AXIS2_PLACEMENT_3D('',#30801,#21551,#21552);
#18913=AXIS2_PLACEMENT_3D('',#30802,#21553,#21554);
#18914=AXIS2_PLACEMENT_3D('',#30804,#21555,#21556);
#18915=AXIS2_PLACEMENT_3D('',#30807,#21558,#21559);
#18916=AXIS2_PLACEMENT_3D('',#30808,#21560,#21561);
#18917=AXIS2_PLACEMENT_3D('',#30810,#21562,#21563);
#18918=AXIS2_PLACEMENT_3D('',#30813,#21565,#21566);
#18919=AXIS2_PLACEMENT_3D('',#30814,#21567,#21568);
#18920=AXIS2_PLACEMENT_3D('',#30816,#21569,#21570);
#18921=AXIS2_PLACEMENT_3D('',#30819,#21572,#21573);
#18922=AXIS2_PLACEMENT_3D('',#30820,#21574,#21575);
#18923=AXIS2_PLACEMENT_3D('',#30823,#21576,#21577);
#18924=AXIS2_PLACEMENT_3D('',#30825,#21578,#21579);
#18925=AXIS2_PLACEMENT_3D('',#30828,#21581,#21582);
#18926=AXIS2_PLACEMENT_3D('',#30829,#21583,#21584);
#18927=AXIS2_PLACEMENT_3D('',#30830,#21585,#21586);
#18928=AXIS2_PLACEMENT_3D('',#30833,#21587,#21588);
#18929=AXIS2_PLACEMENT_3D('',#30840,#21589,#21590);
#18930=AXIS2_PLACEMENT_3D('',#30845,#21591,#21592);
#18931=AXIS2_PLACEMENT_3D('',#30848,#21593,#21594);
#18932=AXIS2_PLACEMENT_3D('',#30859,#21595,#21596);
#18933=AXIS2_PLACEMENT_3D('',#30865,#21597,#21598);
#18934=AXIS2_PLACEMENT_3D('',#30867,#21599,#21600);
#18935=AXIS2_PLACEMENT_3D('',#30874,#21601,#21602);
#18936=AXIS2_PLACEMENT_3D('',#30876,#21603,#21604);
#18937=AXIS2_PLACEMENT_3D('',#30882,#21605,#21606);
#18938=AXIS2_PLACEMENT_3D('',#30883,#21607,#21608);
#18939=AXIS2_PLACEMENT_3D('',#30885,#21609,#21610);
#18940=AXIS2_PLACEMENT_3D('',#30888,#21612,#21613);
#18941=AXIS2_PLACEMENT_3D('',#30889,#21614,#21615);
#18942=AXIS2_PLACEMENT_3D('',#30891,#21616,#21617);
#18943=AXIS2_PLACEMENT_3D('',#30902,#21619,#21620);
#18944=AXIS2_PLACEMENT_3D('',#30911,#21621,#21622);
#18945=AXIS2_PLACEMENT_3D('',#30920,#21623,#21624);
#18946=AXIS2_PLACEMENT_3D('',#30927,#21625,#21626);
#18947=AXIS2_PLACEMENT_3D('',#30930,#21627,#21628);
#18948=AXIS2_PLACEMENT_3D('',#30932,#21629,#21630);
#18949=AXIS2_PLACEMENT_3D('',#30934,#21631,#21632);
#18950=AXIS2_PLACEMENT_3D('',#30937,#21634,#21635);
#18951=AXIS2_PLACEMENT_3D('',#30939,#21636,#21637);
#18952=AXIS2_PLACEMENT_3D('',#30940,#21638,#21639);
#18953=AXIS2_PLACEMENT_3D('',#30941,#21640,#21641);
#18954=AXIS2_PLACEMENT_3D('',#30943,#21642,#21643);
#18955=AXIS2_PLACEMENT_3D('',#30946,#21645,#21646);
#18956=AXIS2_PLACEMENT_3D('',#30947,#21647,#21648);
#18957=AXIS2_PLACEMENT_3D('',#30949,#21649,#21650);
#18958=AXIS2_PLACEMENT_3D('',#30952,#21652,#21653);
#18959=AXIS2_PLACEMENT_3D('',#30953,#21654,#21655);
#18960=AXIS2_PLACEMENT_3D('',#30996,#21658,#21659);
#18961=AXIS2_PLACEMENT_3D('',#31039,#21662,#21663);
#18962=AXIS2_PLACEMENT_3D('',#31042,#21664,#21665);
#18963=AXIS2_PLACEMENT_3D('',#31060,#21667,#21668);
#18964=AXIS2_PLACEMENT_3D('',#31080,#21670,#21671);
#18965=AXIS2_PLACEMENT_3D('',#31104,#21673,#21674);
#18966=AXIS2_PLACEMENT_3D('',#31106,#21676,#21677);
#18967=AXIS2_PLACEMENT_3D('',#31149,#21680,#21681);
#18968=AXIS2_PLACEMENT_3D('',#31152,#21682,#21683);
#18969=AXIS2_PLACEMENT_3D('',#31154,#21684,#21685);
#18970=AXIS2_PLACEMENT_3D('',#31158,#21687,#21688);
#18971=AXIS2_PLACEMENT_3D('',#31160,#21690,#21691);
#18972=AXIS2_PLACEMENT_3D('',#31162,#21692,#21693);
#18973=AXIS2_PLACEMENT_3D('',#31165,#21695,#21696);
#18974=AXIS2_PLACEMENT_3D('',#31166,#21697,#21698);
#18975=AXIS2_PLACEMENT_3D('',#31168,#21699,#21700);
#18976=AXIS2_PLACEMENT_3D('',#31171,#21702,#21703);
#18977=AXIS2_PLACEMENT_3D('',#31172,#21704,#21705);
#18978=AXIS2_PLACEMENT_3D('',#31174,#21706,#21707);
#18979=AXIS2_PLACEMENT_3D('',#31177,#21709,#21710);
#18980=AXIS2_PLACEMENT_3D('',#31178,#21711,#21712);
#18981=AXIS2_PLACEMENT_3D('',#31180,#21713,#21714);
#18982=AXIS2_PLACEMENT_3D('',#31183,#21716,#21717);
#18983=AXIS2_PLACEMENT_3D('',#31184,#21718,#21719);
#18984=AXIS2_PLACEMENT_3D('',#31186,#21720,#21721);
#18985=AXIS2_PLACEMENT_3D('',#31189,#21723,#21724);
#18986=AXIS2_PLACEMENT_3D('',#31190,#21725,#21726);
#18987=AXIS2_PLACEMENT_3D('',#31193,#21727,#21728);
#18988=AXIS2_PLACEMENT_3D('',#31216,#21731,#21732);
#18989=AXIS2_PLACEMENT_3D('',#31219,#21733,#21734);
#18990=AXIS2_PLACEMENT_3D('',#31244,#21737,#21738);
#18991=AXIS2_PLACEMENT_3D('',#31246,#21739,#21740);
#18992=AXIS2_PLACEMENT_3D('',#31250,#21742,#21743);
#18993=AXIS2_PLACEMENT_3D('',#31265,#21745,#21746);
#18994=AXIS2_PLACEMENT_3D('',#31268,#21747,#21748);
#18995=AXIS2_PLACEMENT_3D('',#31274,#21749,#21750);
#18996=AXIS2_PLACEMENT_3D('',#31280,#21751,#21752);
#18997=AXIS2_PLACEMENT_3D('',#31286,#21753,#21754);
#18998=AXIS2_PLACEMENT_3D('',#31292,#21755,#21756);
#18999=AXIS2_PLACEMENT_3D('',#31306,#21758,#21759);
#19000=AXIS2_PLACEMENT_3D('',#31312,#21760,#21761);
#19001=AXIS2_PLACEMENT_3D('',#31318,#21762,#21763);
#19002=AXIS2_PLACEMENT_3D('',#31324,#21764,#21765);
#19003=AXIS2_PLACEMENT_3D('',#31360,#21766,#21767);
#19004=AXIS2_PLACEMENT_3D('',#31363,#21768,#21769);
#19005=AXIS2_PLACEMENT_3D('',#31365,#21770,#21771);
#19006=AXIS2_PLACEMENT_3D('',#31368,#21773,#21774);
#19007=AXIS2_PLACEMENT_3D('',#31369,#21775,#21776);
#19008=AXIS2_PLACEMENT_3D('',#31370,#21777,#21778);
#19009=AXIS2_PLACEMENT_3D('',#31371,#21779,#21780);
#19010=AXIS2_PLACEMENT_3D('',#31374,#21781,#21782);
#19011=AXIS2_PLACEMENT_3D('',#31378,#21784,#21785);
#19012=AXIS2_PLACEMENT_3D('',#31380,#21787,#21788);
#19013=AXIS2_PLACEMENT_3D('',#31383,#21789,#21790);
#19014=AXIS2_PLACEMENT_3D('',#31387,#21792,#21793);
#19015=AXIS2_PLACEMENT_3D('',#31392,#21796,#21797);
#19016=AXIS2_PLACEMENT_3D('',#31394,#21799,#21800);
#19017=AXIS2_PLACEMENT_3D('',#31397,#21802,#21803);
#19018=AXIS2_PLACEMENT_3D('',#31398,#21804,#21805);
#19019=AXIS2_PLACEMENT_3D('',#31400,#21806,#21807);
#19020=AXIS2_PLACEMENT_3D('',#31403,#21809,#21810);
#19021=AXIS2_PLACEMENT_3D('',#31404,#21811,#21812);
#19022=AXIS2_PLACEMENT_3D('',#31406,#21813,#21814);
#19023=AXIS2_PLACEMENT_3D('',#31409,#21816,#21817);
#19024=AXIS2_PLACEMENT_3D('',#31410,#21818,#21819);
#19025=AXIS2_PLACEMENT_3D('',#31412,#21820,#21821);
#19026=AXIS2_PLACEMENT_3D('',#31415,#21823,#21824);
#19027=AXIS2_PLACEMENT_3D('',#31416,#21825,#21826);
#19028=AXIS2_PLACEMENT_3D('',#31418,#21827,#21828);
#19029=AXIS2_PLACEMENT_3D('',#31421,#21830,#21831);
#19030=AXIS2_PLACEMENT_3D('',#31422,#21832,#21833);
#19031=AXIS2_PLACEMENT_3D('',#31424,#21834,#21835);
#19032=AXIS2_PLACEMENT_3D('',#31428,#21837,#21838);
#19033=AXIS2_PLACEMENT_3D('',#31432,#21840,#21841);
#19034=AXIS2_PLACEMENT_3D('',#31435,#21843,#21844);
#19035=AXIS2_PLACEMENT_3D('',#31437,#21845,#21846);
#19036=AXIS2_PLACEMENT_3D('',#31440,#21848,#21849);
#19037=AXIS2_PLACEMENT_3D('',#31441,#21850,#21851);
#19038=AXIS2_PLACEMENT_3D('',#31443,#21852,#21853);
#19039=AXIS2_PLACEMENT_3D('',#31446,#21855,#21856);
#19040=AXIS2_PLACEMENT_3D('',#31447,#21857,#21858);
#19041=AXIS2_PLACEMENT_3D('',#31449,#21859,#21860);
#19042=AXIS2_PLACEMENT_3D('',#31452,#21862,#21863);
#19043=AXIS2_PLACEMENT_3D('',#31453,#21864,#21865);
#19044=AXIS2_PLACEMENT_3D('',#31456,#21867,#21868);
#19045=AXIS2_PLACEMENT_3D('',#31457,#21869,#21870);
#19046=AXIS2_PLACEMENT_3D('',#31459,#21871,#21872);
#19047=AXIS2_PLACEMENT_3D('',#31462,#21874,#21875);
#19048=AXIS2_PLACEMENT_3D('',#31463,#21876,#21877);
#19049=AXIS2_PLACEMENT_3D('',#31465,#21878,#21879);
#19050=AXIS2_PLACEMENT_3D('',#31468,#21881,#21882);
#19051=AXIS2_PLACEMENT_3D('',#31469,#21883,#21884);
#19052=AXIS2_PLACEMENT_3D('',#31471,#21885,#21886);
#19053=AXIS2_PLACEMENT_3D('',#31474,#21888,#21889);
#19054=AXIS2_PLACEMENT_3D('',#31475,#21890,#21891);
#19055=AXIS2_PLACEMENT_3D('',#31477,#21892,#21893);
#19056=AXIS2_PLACEMENT_3D('',#31480,#21895,#21896);
#19057=AXIS2_PLACEMENT_3D('',#31481,#21897,#21898);
#19058=AXIS2_PLACEMENT_3D('',#31483,#21899,#21900);
#19059=AXIS2_PLACEMENT_3D('',#31486,#21902,#21903);
#19060=AXIS2_PLACEMENT_3D('',#31487,#21904,#21905);
#19061=AXIS2_PLACEMENT_3D('',#31489,#21906,#21907);
#19062=AXIS2_PLACEMENT_3D('',#31492,#21909,#21910);
#19063=AXIS2_PLACEMENT_3D('',#31493,#21911,#21912);
#19064=AXIS2_PLACEMENT_3D('',#31496,#21913,#21914);
#19065=AXIS2_PLACEMENT_3D('',#31500,#21916,#21917);
#19066=AXIS2_PLACEMENT_3D('',#31502,#21919,#21920);
#19067=AXIS2_PLACEMENT_3D('',#31506,#21922,#21923);
#19068=AXIS2_PLACEMENT_3D('',#31507,#21924,#21925);
#19069=AXIS2_PLACEMENT_3D('',#31508,#21926,#21927);
#19070=AXIS2_PLACEMENT_3D('',#31511,#21928,#21929);
#19071=AXIS2_PLACEMENT_3D('',#31515,#21931,#21932);
#19072=AXIS2_PLACEMENT_3D('',#31517,#21934,#21935);
#19073=AXIS2_PLACEMENT_3D('',#31520,#21936,#21937);
#19074=AXIS2_PLACEMENT_3D('',#31521,#21938,#21939);
#19075=AXIS2_PLACEMENT_3D('',#31523,#21941,#21942);
#19076=AXIS2_PLACEMENT_3D('',#31526,#21943,#21944);
#19077=AXIS2_PLACEMENT_3D('',#31527,#21945,#21946);
#19078=AXIS2_PLACEMENT_3D('',#31529,#21948,#21949);
#19079=AXIS2_PLACEMENT_3D('',#31550,#21950,#21951);
#19080=AXIS2_PLACEMENT_3D('',#31577,#21952,#21953);
#19081=AXIS2_PLACEMENT_3D('',#31595,#21955,#21956);
#19082=AXIS2_PLACEMENT_3D('',#31613,#21958,#21959);
#19083=AXIS2_PLACEMENT_3D('',#31638,#21960,#21961);
#19084=AXIS2_PLACEMENT_3D('',#31645,#21962,#21963);
#19085=AXIS2_PLACEMENT_3D('',#31647,#21964,#21965);
#19086=AXIS2_PLACEMENT_3D('',#31650,#21967,#21968);
#19087=AXIS2_PLACEMENT_3D('',#31651,#21969,#21970);
#19088=AXIS2_PLACEMENT_3D('',#31653,#21971,#21972);
#19089=AXIS2_PLACEMENT_3D('',#31656,#21974,#21975);
#19090=AXIS2_PLACEMENT_3D('',#31657,#21976,#21977);
#19091=AXIS2_PLACEMENT_3D('',#31660,#21979,#21980);
#19092=AXIS2_PLACEMENT_3D('',#31661,#21981,#21982);
#19093=AXIS2_PLACEMENT_3D('',#31663,#21983,#21984);
#19094=AXIS2_PLACEMENT_3D('',#31667,#21986,#21987);
#19095=AXIS2_PLACEMENT_3D('',#31668,#21988,#21989);
#19096=AXIS2_PLACEMENT_3D('',#31669,#21990,#21991);
#19097=AXIS2_PLACEMENT_3D('',#31672,#21992,#21993);
#19098=AXIS2_PLACEMENT_3D('',#31676,#21995,#21996);
#19099=AXIS2_PLACEMENT_3D('',#31678,#21998,#21999);
#19100=AXIS2_PLACEMENT_3D('',#31691,#22001,#22002);
#19101=AXIS2_PLACEMENT_3D('',#31708,#22003,#22004);
#19102=AXIS2_PLACEMENT_3D('',#31840,#22009,#22010);
#19103=AXIS2_PLACEMENT_3D('',#31916,#22013,#22014);
#19104=AXIS2_PLACEMENT_3D('',#31990,#22017,#22018);
#19105=AXIS2_PLACEMENT_3D('',#32011,#22019,#22020);
#19106=AXIS2_PLACEMENT_3D('',#32022,#22021,#22022);
#19107=AXIS2_PLACEMENT_3D('',#32035,#22029,#22030);
#19108=AXIS2_PLACEMENT_3D('',#32048,#22037,#22038);
#19109=AXIS2_PLACEMENT_3D('',#32061,#22045,#22046);
#19110=AXIS2_PLACEMENT_3D('',#32074,#22053,#22054);
#19111=AXIS2_PLACEMENT_3D('',#32077,#22055,#22056);
#19112=AXIS2_PLACEMENT_3D('',#32081,#22058,#22059);
#19113=AXIS2_PLACEMENT_3D('',#32083,#22060,#22061);
#19114=AXIS2_PLACEMENT_3D('',#32085,#22062,#22063);
#19115=AXIS2_PLACEMENT_3D('',#32088,#22065,#22066);
#19116=AXIS2_PLACEMENT_3D('',#32090,#22067,#22068);
#19117=AXIS2_PLACEMENT_3D('',#32094,#22070,#22071);
#19118=AXIS2_PLACEMENT_3D('',#32096,#22072,#22073);
#19119=AXIS2_PLACEMENT_3D('',#32098,#22074,#22075);
#19120=AXIS2_PLACEMENT_3D('',#32102,#22077,#22078);
#19121=AXIS2_PLACEMENT_3D('',#32103,#22079,#22080);
#19122=AXIS2_PLACEMENT_3D('',#32104,#22081,#22082);
#19123=AXIS2_PLACEMENT_3D('',#32117,#22089,#22090);
#19124=AXIS2_PLACEMENT_3D('',#32130,#22097,#22098);
#19125=AXIS2_PLACEMENT_3D('',#32136,#22102,#22103);
#19126=AXIS2_PLACEMENT_3D('',#32140,#22106,#22107);
#19127=AXIS2_PLACEMENT_3D('',#32144,#22110,#22111);
#19128=AXIS2_PLACEMENT_3D('',#32148,#22114,#22115);
#19129=AXIS2_PLACEMENT_3D('',#32152,#22118,#22119);
#19130=AXIS2_PLACEMENT_3D('',#32154,#22121,#22122);
#19131=AXIS2_PLACEMENT_3D('',#32164,#22127,#22128);
#19132=AXIS2_PLACEMENT_3D('',#32165,#22129,#22130);
#19133=AXIS2_PLACEMENT_3D('',#32169,#22132,#22133);
#19134=AXIS2_PLACEMENT_3D('',#32170,#22134,#22135);
#19135=AXIS2_PLACEMENT_3D('',#32171,#22136,#22137);
#19136=AXIS2_PLACEMENT_3D('',#32178,#22141,#22142);
#19137=AXIS2_PLACEMENT_3D('',#32179,#22143,#22144);
#19138=AXIS2_PLACEMENT_3D('',#32185,#22148,#22149);
#19139=AXIS2_PLACEMENT_3D('',#32189,#22152,#22153);
#19140=AXIS2_PLACEMENT_3D('',#32193,#22156,#22157);
#19141=AXIS2_PLACEMENT_3D('',#32197,#22160,#22161);
#19142=AXIS2_PLACEMENT_3D('',#32201,#22164,#22165);
#19143=AXIS2_PLACEMENT_3D('',#32203,#22167,#22168);
#19144=AXIS2_PLACEMENT_3D('',#32213,#22173,#22174);
#19145=AXIS2_PLACEMENT_3D('',#32214,#22175,#22176);
#19146=AXIS2_PLACEMENT_3D('',#32218,#22178,#22179);
#19147=AXIS2_PLACEMENT_3D('',#32219,#22180,#22181);
#19148=AXIS2_PLACEMENT_3D('',#32220,#22182,#22183);
#19149=AXIS2_PLACEMENT_3D('',#32227,#22187,#22188);
#19150=AXIS2_PLACEMENT_3D('',#32228,#22189,#22190);
#19151=AXIS2_PLACEMENT_3D('',#32234,#22194,#22195);
#19152=AXIS2_PLACEMENT_3D('',#32238,#22198,#22199);
#19153=AXIS2_PLACEMENT_3D('',#32242,#22202,#22203);
#19154=AXIS2_PLACEMENT_3D('',#32246,#22206,#22207);
#19155=AXIS2_PLACEMENT_3D('',#32250,#22210,#22211);
#19156=AXIS2_PLACEMENT_3D('',#32252,#22213,#22214);
#19157=AXIS2_PLACEMENT_3D('',#32262,#22219,#22220);
#19158=AXIS2_PLACEMENT_3D('',#32263,#22221,#22222);
#19159=AXIS2_PLACEMENT_3D('',#32267,#22224,#22225);
#19160=AXIS2_PLACEMENT_3D('',#32268,#22226,#22227);
#19161=AXIS2_PLACEMENT_3D('',#32269,#22228,#22229);
#19162=AXIS2_PLACEMENT_3D('',#32276,#22233,#22234);
#19163=AXIS2_PLACEMENT_3D('',#32277,#22235,#22236);
#19164=AXIS2_PLACEMENT_3D('',#32284,#22240,#22241);
#19165=AXIS2_PLACEMENT_3D('',#32289,#22245,#22246);
#19166=AXIS2_PLACEMENT_3D('',#32295,#22250,#22251);
#19167=AXIS2_PLACEMENT_3D('',#32299,#22254,#22255);
#19168=AXIS2_PLACEMENT_3D('',#32303,#22258,#22259);
#19169=AXIS2_PLACEMENT_3D('',#32307,#22262,#22263);
#19170=AXIS2_PLACEMENT_3D('',#32311,#22266,#22267);
#19171=AXIS2_PLACEMENT_3D('',#32313,#22269,#22270);
#19172=AXIS2_PLACEMENT_3D('',#32320,#22274,#22275);
#19173=AXIS2_PLACEMENT_3D('',#32321,#22276,#22277);
#19174=AXIS2_PLACEMENT_3D('',#32324,#22279,#22280);
#19175=AXIS2_PLACEMENT_3D('',#32325,#22281,#22282);
#19176=AXIS2_PLACEMENT_3D('',#32330,#22285,#22286);
#19177=AXIS2_PLACEMENT_3D('',#32331,#22287,#22288);
#19178=AXIS2_PLACEMENT_3D('',#32336,#22291,#22292);
#19179=AXIS2_PLACEMENT_3D('',#32337,#22293,#22294);
#19180=AXIS2_PLACEMENT_3D('',#32341,#22297,#22298);
#19181=AXIS2_PLACEMENT_3D('',#32344,#22300,#22301);
#19182=AXIS2_PLACEMENT_3D('',#32345,#22302,#22303);
#19183=AXIS2_PLACEMENT_3D('',#32348,#22305,#22306);
#19184=AXIS2_PLACEMENT_3D('',#32349,#22307,#22308);
#19185=AXIS2_PLACEMENT_3D('',#32352,#22310,#22311);
#19186=AXIS2_PLACEMENT_3D('',#32353,#22312,#22313);
#19187=AXIS2_PLACEMENT_3D('',#32357,#22316,#22317);
#19188=AXIS2_PLACEMENT_3D('',#32360,#22319,#22320);
#19189=AXIS2_PLACEMENT_3D('',#32361,#22321,#22322);
#19190=AXIS2_PLACEMENT_3D('',#32364,#22324,#22325);
#19191=AXIS2_PLACEMENT_3D('',#32365,#22326,#22327);
#19192=AXIS2_PLACEMENT_3D('',#32368,#22329,#22330);
#19193=AXIS2_PLACEMENT_3D('',#32369,#22331,#22332);
#19194=AXIS2_PLACEMENT_3D('',#32373,#22335,#22336);
#19195=AXIS2_PLACEMENT_3D('',#32374,#22337,#22338);
#19196=AXIS2_PLACEMENT_3D('',#32375,#22339,#22340);
#19197=AXIS2_PLACEMENT_3D('',#32378,#22342,#22343);
#19198=AXIS2_PLACEMENT_3D('',#32379,#22344,#22345);
#19199=AXIS2_PLACEMENT_3D('',#32383,#22348,#22349);
#19200=AXIS2_PLACEMENT_3D('',#32386,#22351,#22352);
#19201=AXIS2_PLACEMENT_3D('',#32387,#22353,#22354);
#19202=AXIS2_PLACEMENT_3D('',#32388,#22355,#22356);
#19203=AXIS2_PLACEMENT_3D('',#32389,#22357,#22358);
#19204=AXIS2_PLACEMENT_3D('',#32394,#22361,#22362);
#19205=AXIS2_PLACEMENT_3D('',#32395,#22363,#22364);
#19206=AXIS2_PLACEMENT_3D('',#32398,#22366,#22367);
#19207=AXIS2_PLACEMENT_3D('',#32399,#22368,#22369);
#19208=AXIS2_PLACEMENT_3D('',#32402,#22371,#22372);
#19209=AXIS2_PLACEMENT_3D('',#32403,#22373,#22374);
#19210=AXIS2_PLACEMENT_3D('',#32406,#22376,#22377);
#19211=AXIS2_PLACEMENT_3D('',#32407,#22378,#22379);
#19212=AXIS2_PLACEMENT_3D('',#32410,#22381,#22382);
#19213=AXIS2_PLACEMENT_3D('',#32411,#22383,#22384);
#19214=AXIS2_PLACEMENT_3D('',#32412,#22385,#22386);
#19215=AXIS2_PLACEMENT_3D('',#32413,#22387,#22388);
#19216=AXIS2_PLACEMENT_3D('',#32418,#22391,#22392);
#19217=AXIS2_PLACEMENT_3D('',#32419,#22393,#22394);
#19218=AXIS2_PLACEMENT_3D('',#32422,#22396,#22397);
#19219=AXIS2_PLACEMENT_3D('',#32423,#22398,#22399);
#19220=AXIS2_PLACEMENT_3D('',#32426,#22401,#22402);
#19221=AXIS2_PLACEMENT_3D('',#32427,#22403,#22404);
#19222=AXIS2_PLACEMENT_3D('',#32430,#22406,#22407);
#19223=AXIS2_PLACEMENT_3D('',#32431,#22408,#22409);
#19224=AXIS2_PLACEMENT_3D('',#32434,#22411,#22412);
#19225=AXIS2_PLACEMENT_3D('',#32435,#22413,#22414);
#19226=AXIS2_PLACEMENT_3D('',#32436,#22415,#22416);
#19227=AXIS2_PLACEMENT_3D('',#32437,#22417,#22418);
#19228=AXIS2_PLACEMENT_3D('',#32439,#22420,#22421);
#19229=AXIS2_PLACEMENT_3D('',#32441,#22423,#22424);
#19230=AXIS2_PLACEMENT_3D('',#32444,#22425,#22426);
#19231=AXIS2_PLACEMENT_3D('',#32447,#22429,#22430);
#19232=AXIS2_PLACEMENT_3D('',#32449,#22432,#22433);
#19233=AXIS2_PLACEMENT_3D('',#32453,#22435,#22436);
#19234=AXIS2_PLACEMENT_3D('',#32455,#22438,#22439);
#19235=AXIS2_PLACEMENT_3D('',#32459,#22441,#22442);
#19236=AXIS2_PLACEMENT_3D('',#32461,#22444,#22445);
#19237=AXIS2_PLACEMENT_3D('',#32463,#22447,#22448);
#19238=AXIS2_PLACEMENT_3D('',#32467,#22450,#22451);
#19239=AXIS2_PLACEMENT_3D('',#32469,#22453,#22454);
#19240=AXIS2_PLACEMENT_3D('',#32488,#22457,#22458);
#19241=AXIS2_PLACEMENT_3D('',#32490,#22459,#22460);
#19242=AXIS2_PLACEMENT_3D('',#32499,#22462,#22463);
#19243=AXIS2_PLACEMENT_3D('',#32515,#22465,#22466);
#19244=AXIS2_PLACEMENT_3D('',#32526,#22469,#22470);
#19245=AXIS2_PLACEMENT_3D('',#32528,#22471,#22472);
#19246=AXIS2_PLACEMENT_3D('',#32537,#22474,#22475);
#19247=AXIS2_PLACEMENT_3D('',#32545,#22477,#22478);
#19248=AXIS2_PLACEMENT_3D('',#32549,#22481,#22482);
#19249=AXIS2_PLACEMENT_3D('',#32551,#22483,#22484);
#19250=AXIS2_PLACEMENT_3D('',#32553,#22486,#22487);
#19251=AXIS2_PLACEMENT_3D('',#32555,#22489,#22490);
#19252=AXIS2_PLACEMENT_3D('',#32578,#22493,#22494);
#19253=AXIS2_PLACEMENT_3D('',#32580,#22495,#22496);
#19254=AXIS2_PLACEMENT_3D('',#32589,#22498,#22499);
#19255=AXIS2_PLACEMENT_3D('',#32605,#22501,#22502);
#19256=AXIS2_PLACEMENT_3D('',#32626,#22503,#22504);
#19257=AXIS2_PLACEMENT_3D('',#32668,#22505,#22506);
#19258=AXIS2_PLACEMENT_3D('',#32682,#22507,#22508);
#19259=AXIS2_PLACEMENT_3D('',#32733,#22509,#22510);
#19260=AXIS2_PLACEMENT_3D('',#32744,#22511,#22512);
#19261=AXIS2_PLACEMENT_3D('',#32795,#22513,#22514);
#19262=AXIS2_PLACEMENT_3D('',#32831,#22515,#22516);
#19263=AXIS2_PLACEMENT_3D('',#32881,#22517,#22518);
#19264=AXIS2_PLACEMENT_3D('',#32882,#22519,#22520);
#19265=AXIS2_PLACEMENT_3D('',#32883,#22521,#22522);
#19266=AXIS2_PLACEMENT_3D('',#32884,#22523,#22524);
#19267=AXIS2_PLACEMENT_3D('',#32887,#22525,#22526);
#19268=AXIS2_PLACEMENT_3D('',#32890,#22529,#22530);
#19269=AXIS2_PLACEMENT_3D('',#32894,#22533,#22534);
#19270=AXIS2_PLACEMENT_3D('',#32896,#22535,#22536);
#19271=AXIS2_PLACEMENT_3D('',#32898,#22538,#22539);
#19272=AXIS2_PLACEMENT_3D('',#32902,#22542,#22543);
#19273=AXIS2_PLACEMENT_3D('',#32904,#22544,#22545);
#19274=AXIS2_PLACEMENT_3D('',#32906,#22547,#22548);
#19275=AXIS2_PLACEMENT_3D('',#32910,#22551,#22552);
#19276=AXIS2_PLACEMENT_3D('',#32912,#22553,#22554);
#19277=AXIS2_PLACEMENT_3D('',#32914,#22556,#22557);
#19278=AXIS2_PLACEMENT_3D('',#33033,#22563,#22564);
#19279=AXIS2_PLACEMENT_3D('',#33036,#22565,#22566);
#19280=AXIS2_PLACEMENT_3D('',#33083,#22569,#22570);
#19281=AXIS2_PLACEMENT_3D('',#33086,#22571,#22572);
#19282=AXIS2_PLACEMENT_3D('',#33135,#22575,#22576);
#19283=AXIS2_PLACEMENT_3D('',#33138,#22577,#22578);
#19284=AXIS2_PLACEMENT_3D('',#33187,#22581,#22582);
#19285=AXIS2_PLACEMENT_3D('',#33190,#22583,#22584);
#19286=AXIS2_PLACEMENT_3D('',#33326,#22585,#22586);
#19287=AXIS2_PLACEMENT_3D('',#33389,#22587,#22588);
#19288=AXIS2_PLACEMENT_3D('',#33390,#22589,#22590);
#19289=AXIS2_PLACEMENT_3D('',#33416,#22592,#22593);
#19290=AXIS2_PLACEMENT_3D('',#33441,#22596,#22597);
#19291=AXIS2_PLACEMENT_3D('',#33542,#22600,#22601);
#19292=AXIS2_PLACEMENT_3D('',#33554,#22602,#22603);
#19293=AXIS2_PLACEMENT_3D('',#33557,#22604,#22605);
#19294=AXIS2_PLACEMENT_3D('',#33714,#22608,#22609);
#19295=AXIS2_PLACEMENT_3D('',#33717,#22610,#22611);
#19296=AXIS2_PLACEMENT_3D('',#33874,#22614,#22615);
#19297=AXIS2_PLACEMENT_3D('',#33877,#22616,#22617);
#19298=AXIS2_PLACEMENT_3D('',#34034,#22620,#22621);
#19299=AXIS2_PLACEMENT_3D('',#34037,#22622,#22623);
#19300=AXIS2_PLACEMENT_3D('',#35987,#22626,#22627);
#19301=AXIS2_PLACEMENT_3D('',#35988,#22628,#22629);
#19302=AXIS2_PLACEMENT_3D('',#35991,#22630,#22631);
#19303=AXIS2_PLACEMENT_3D('',#36058,#22632,#22633);
#19304=AXIS2_PLACEMENT_3D('',#36061,#22634,#22635);
#19305=AXIS2_PLACEMENT_3D('',#36062,#22636,#22637);
#19306=AXIS2_PLACEMENT_3D('',#36105,#22640,#22641);
#19307=AXIS2_PLACEMENT_3D('',#36108,#22642,#22643);
#19308=AXIS2_PLACEMENT_3D('',#36157,#22646,#22647);
#19309=AXIS2_PLACEMENT_3D('',#36160,#22648,#22649);
#19310=AXIS2_PLACEMENT_3D('',#36229,#22652,#22653);
#19311=AXIS2_PLACEMENT_3D('',#36234,#22655,#22656);
#19312=AXIS2_PLACEMENT_3D('',#36238,#22658,#22659);
#19313=AXIS2_PLACEMENT_3D('',#36242,#22661,#22662);
#19314=AXIS2_PLACEMENT_3D('',#36245,#22664,#22665);
#19315=AXIS2_PLACEMENT_3D('',#36246,#22666,#22667);
#19316=AXIS2_PLACEMENT_3D('',#36249,#22668,#22669);
#19317=AXIS2_PLACEMENT_3D('',#36252,#22672,#22673);
#19318=AXIS2_PLACEMENT_3D('',#36254,#22674,#22675);
#19319=AXIS2_PLACEMENT_3D('',#36256,#22677,#22678);
#19320=AXIS2_PLACEMENT_3D('',#36258,#22679,#22680);
#19321=AXIS2_PLACEMENT_3D('',#36260,#22682,#22683);
#19322=AXIS2_PLACEMENT_3D('',#36263,#22685,#22686);
#19323=AXIS2_PLACEMENT_3D('',#36264,#22687,#22688);
#19324=AXIS2_PLACEMENT_3D('',#36266,#22689,#22690);
#19325=AXIS2_PLACEMENT_3D('',#36268,#22692,#22693);
#19326=AXIS2_PLACEMENT_3D('',#36270,#22694,#22695);
#19327=AXIS2_PLACEMENT_3D('',#36272,#22697,#22698);
#19328=AXIS2_PLACEMENT_3D('',#36273,#22699,#22700);
#19329=AXIS2_PLACEMENT_3D('',#36274,#22701,#22702);
#19330=AXIS2_PLACEMENT_3D('',#36276,#22703,#22704);
#19331=AXIS2_PLACEMENT_3D('',#36278,#22706,#22707);
#19332=AXIS2_PLACEMENT_3D('',#36280,#22708,#22709);
#19333=AXIS2_PLACEMENT_3D('',#36282,#22711,#22712);
#19334=AXIS2_PLACEMENT_3D('',#36284,#22713,#22714);
#19335=AXIS2_PLACEMENT_3D('',#36289,#22715,#22716);
#19336=AXIS2_PLACEMENT_3D('',#36292,#22718,#22719);
#19337=AXIS2_PLACEMENT_3D('',#36293,#22720,#22721);
#19338=AXIS2_PLACEMENT_3D('',#36295,#22722,#22723);
#19339=AXIS2_PLACEMENT_3D('',#36297,#22725,#22726);
#19340=AXIS2_PLACEMENT_3D('',#36299,#22727,#22728);
#19341=AXIS2_PLACEMENT_3D('',#36301,#22730,#22731);
#19342=AXIS2_PLACEMENT_3D('',#36303,#22732,#22733);
#19343=AXIS2_PLACEMENT_3D('',#36305,#22735,#22736);
#19344=AXIS2_PLACEMENT_3D('',#36306,#22737,#22738);
#19345=AXIS2_PLACEMENT_3D('',#36307,#22739,#22740);
#19346=AXIS2_PLACEMENT_3D('',#36313,#22744,#22745);
#19347=AXIS2_PLACEMENT_3D('',#36319,#22749,#22750);
#19348=AXIS2_PLACEMENT_3D('',#36328,#22751,#22752);
#19349=AXIS2_PLACEMENT_3D('',#36335,#22753,#22754);
#19350=AXIS2_PLACEMENT_3D('',#36341,#22758,#22759);
#19351=AXIS2_PLACEMENT_3D('',#36350,#22760,#22761);
#19352=AXIS2_PLACEMENT_3D('',#36357,#22762,#22763);
#19353=AXIS2_PLACEMENT_3D('',#36366,#22764,#22765);
#19354=AXIS2_PLACEMENT_3D('',#36375,#22767,#22768);
#19355=AXIS2_PLACEMENT_3D('',#36386,#22770,#22771);
#19356=AXIS2_PLACEMENT_3D('',#36393,#22772,#22773);
#19357=AXIS2_PLACEMENT_3D('',#36454,#22776,#22777);
#19358=AXIS2_PLACEMENT_3D('',#36518,#22778,#22779);
#19359=AXIS2_PLACEMENT_3D('',#36613,#22781,#22782);
#19360=AXIS2_PLACEMENT_3D('',#36666,#22784,#22785);
#19361=AXIS2_PLACEMENT_3D('',#36761,#22787,#22788);
#19362=AXIS2_PLACEMENT_3D('',#36832,#22789,#22790);
#19363=AXIS2_PLACEMENT_3D('',#36885,#22792,#22793);
#19364=AXIS2_PLACEMENT_3D('',#36981,#22795,#22796);
#19365=AXIS2_PLACEMENT_3D('',#37031,#22797,#22798);
#19366=AXIS2_PLACEMENT_3D('',#37047,#22799,#22800);
#19367=AXIS2_PLACEMENT_3D('',#37098,#22801,#22802);
#19368=AXIS2_PLACEMENT_3D('',#37102,#22804,#22805);
#19369=AXIS2_PLACEMENT_3D('',#37166,#22806,#22807);
#19370=AXIS2_PLACEMENT_3D('',#37261,#22809,#22810);
#19371=AXIS2_PLACEMENT_3D('',#37262,#22811,#22812);
#19372=AXIS2_PLACEMENT_3D('',#37263,#22813,#22814);
#19373=AXIS2_PLACEMENT_3D('',#37265,#22815,#22816);
#19374=AXIS2_PLACEMENT_3D('',#37267,#22817,#22818);
#19375=AXIS2_PLACEMENT_3D('',#37268,#22819,#22820);
#19376=AXIS2_PLACEMENT_3D('',#37270,#22821,#22822);
#19377=AXIS2_PLACEMENT_3D('',#37272,#22823,#22824);
#19378=AXIS2_PLACEMENT_3D('',#37273,#22825,#22826);
#19379=AXIS2_PLACEMENT_3D('',#37275,#22827,#22828);
#19380=AXIS2_PLACEMENT_3D('',#37277,#22829,#22830);
#19381=AXIS2_PLACEMENT_3D('',#37278,#22831,#22832);
#19382=AXIS2_PLACEMENT_3D('',#37279,#22833,#22834);
#19383=AXIS2_PLACEMENT_3D('',#37280,#22835,#22836);
#19384=AXIS2_PLACEMENT_3D('',#37293,#22843,#22844);
#19385=AXIS2_PLACEMENT_3D('',#37306,#22851,#22852);
#19386=AXIS2_PLACEMENT_3D('',#37308,#22854,#22855);
#19387=AXIS2_PLACEMENT_3D('',#37310,#22857,#22858);
#19388=AXIS2_PLACEMENT_3D('',#37312,#22860,#22861);
#19389=AXIS2_PLACEMENT_3D('',#37314,#22863,#22864);
#19390=AXIS2_PLACEMENT_3D('',#37317,#22865,#22866);
#19391=AXIS2_PLACEMENT_3D('',#37323,#22868,#22869);
#19392=AXIS2_PLACEMENT_3D('',#37327,#22872,#22873);
#19393=AXIS2_PLACEMENT_3D('',#37331,#22876,#22877);
#19394=AXIS2_PLACEMENT_3D('',#37338,#22879,#22880);
#19395=AXIS2_PLACEMENT_3D('',#37340,#22881,#22882);
#19396=AXIS2_PLACEMENT_3D('',#37342,#22884,#22885);
#19397=AXIS2_PLACEMENT_3D('',#37345,#22887,#22888);
#19398=AXIS2_PLACEMENT_3D('',#37346,#22889,#22890);
#19399=AXIS2_PLACEMENT_3D('',#37348,#22891,#22892);
#19400=AXIS2_PLACEMENT_3D('',#37353,#22893,#22894);
#19401=AXIS2_PLACEMENT_3D('',#37357,#22897,#22898);
#19402=AXIS2_PLACEMENT_3D('',#37361,#22901,#22902);
#19403=AXIS2_PLACEMENT_3D('',#37368,#22904,#22905);
#19404=AXIS2_PLACEMENT_3D('',#37369,#22906,#22907);
#19405=AXIS2_PLACEMENT_3D('',#37370,#22908,#22909);
#19406=AXIS2_PLACEMENT_3D('',#37372,#22910,#22911);
#19407=AXIS2_PLACEMENT_3D('',#37377,#22912,#22913);
#19408=AXIS2_PLACEMENT_3D('',#37381,#22916,#22917);
#19409=AXIS2_PLACEMENT_3D('',#37385,#22920,#22921);
#19410=AXIS2_PLACEMENT_3D('',#37392,#22923,#22924);
#19411=AXIS2_PLACEMENT_3D('',#37394,#22925,#22926);
#19412=AXIS2_PLACEMENT_3D('',#37396,#22928,#22929);
#19413=AXIS2_PLACEMENT_3D('',#37399,#22931,#22932);
#19414=AXIS2_PLACEMENT_3D('',#37400,#22933,#22934);
#19415=AXIS2_PLACEMENT_3D('',#37402,#22935,#22936);
#19416=AXIS2_PLACEMENT_3D('',#37407,#22937,#22938);
#19417=AXIS2_PLACEMENT_3D('',#37411,#22941,#22942);
#19418=AXIS2_PLACEMENT_3D('',#37415,#22945,#22946);
#19419=AXIS2_PLACEMENT_3D('',#37422,#22948,#22949);
#19420=AXIS2_PLACEMENT_3D('',#37424,#22950,#22951);
#19421=AXIS2_PLACEMENT_3D('',#37426,#22953,#22954);
#19422=AXIS2_PLACEMENT_3D('',#37427,#22955,#22956);
#19423=AXIS2_PLACEMENT_3D('',#37428,#22957,#22958);
#19424=AXIS2_PLACEMENT_3D('',#37434,#22962,#22963);
#19425=AXIS2_PLACEMENT_3D('',#37438,#22966,#22967);
#19426=AXIS2_PLACEMENT_3D('',#37442,#22970,#22971);
#19427=AXIS2_PLACEMENT_3D('',#37446,#22974,#22975);
#19428=AXIS2_PLACEMENT_3D('',#37450,#22978,#22979);
#19429=AXIS2_PLACEMENT_3D('',#37452,#22981,#22982);
#19430=AXIS2_PLACEMENT_3D('',#37458,#22986,#22987);
#19431=AXIS2_PLACEMENT_3D('',#37462,#22990,#22991);
#19432=AXIS2_PLACEMENT_3D('',#37466,#22994,#22995);
#19433=AXIS2_PLACEMENT_3D('',#37470,#22998,#22999);
#19434=AXIS2_PLACEMENT_3D('',#37474,#23002,#23003);
#19435=AXIS2_PLACEMENT_3D('',#37476,#23005,#23006);
#19436=AXIS2_PLACEMENT_3D('',#37479,#23007,#23008);
#19437=AXIS2_PLACEMENT_3D('',#37483,#23010,#23011);
#19438=AXIS2_PLACEMENT_3D('',#37485,#23013,#23014);
#19439=AXIS2_PLACEMENT_3D('',#37488,#23015,#23016);
#19440=AXIS2_PLACEMENT_3D('',#37492,#23018,#23019);
#19441=AXIS2_PLACEMENT_3D('',#37494,#23021,#23022);
#19442=AXIS2_PLACEMENT_3D('',#37503,#23027,#23028);
#19443=AXIS2_PLACEMENT_3D('',#37508,#23030,#23031);
#19444=AXIS2_PLACEMENT_3D('',#37513,#23035,#23036);
#19445=AXIS2_PLACEMENT_3D('',#37518,#23039,#23040);
#19446=AXIS2_PLACEMENT_3D('',#37519,#23041,#23042);
#19447=AXIS2_PLACEMENT_3D('',#37522,#23043,#23044);
#19448=AXIS2_PLACEMENT_3D('',#37526,#23046,#23047);
#19449=AXIS2_PLACEMENT_3D('',#37528,#23049,#23050);
#19450=AXIS2_PLACEMENT_3D('',#37531,#23051,#23052);
#19451=AXIS2_PLACEMENT_3D('',#37535,#23054,#23055);
#19452=AXIS2_PLACEMENT_3D('',#37537,#23057,#23058);
#19453=AXIS2_PLACEMENT_3D('',#37540,#23059,#23060);
#19454=AXIS2_PLACEMENT_3D('',#37544,#23062,#23063);
#19455=AXIS2_PLACEMENT_3D('',#37546,#23065,#23066);
#19456=AXIS2_PLACEMENT_3D('',#37555,#23073,#23074);
#19457=AXIS2_PLACEMENT_3D('',#37558,#23077,#23078);
#19458=AXIS2_PLACEMENT_3D('',#37561,#23079,#23080);
#19459=AXIS2_PLACEMENT_3D('',#37564,#23083,#23084);
#19460=AXIS2_PLACEMENT_3D('',#37565,#23085,#23086);
#19461=AXIS2_PLACEMENT_3D('',#37566,#23087,#23088);
#19462=AXIS2_PLACEMENT_3D('',#37572,#23092,#23093);
#19463=AXIS2_PLACEMENT_3D('',#37578,#23097,#23098);
#19464=AXIS2_PLACEMENT_3D('',#37582,#23100,#23101);
#19465=AXIS2_PLACEMENT_3D('',#37590,#23105,#23106);
#19466=AXIS2_PLACEMENT_3D('',#37592,#23108,#23109);
#19467=AXIS2_PLACEMENT_3D('',#37597,#23111,#23112);
#19468=AXIS2_PLACEMENT_3D('',#37600,#23114,#23115);
#19469=AXIS2_PLACEMENT_3D('',#37601,#23116,#23117);
#19470=AXIS2_PLACEMENT_3D('',#37609,#23122,#23123);
#19471=AXIS2_PLACEMENT_3D('',#37612,#23126,#23127);
#19472=AXIS2_PLACEMENT_3D('',#37617,#23129,#23130);
#19473=AXIS2_PLACEMENT_3D('',#37620,#23133,#23134);
#19474=AXIS2_PLACEMENT_3D('',#37624,#23137,#23138);
#19475=AXIS2_PLACEMENT_3D('',#37632,#23143,#23144);
#19476=AXIS2_PLACEMENT_3D('',#37638,#23148,#23149);
#19477=AXIS2_PLACEMENT_3D('',#37644,#23153,#23154);
#19478=AXIS2_PLACEMENT_3D('',#37648,#23156,#23157);
#19479=AXIS2_PLACEMENT_3D('',#37650,#23159,#23160);
#19480=AXIS2_PLACEMENT_3D('',#37655,#23162,#23163);
#19481=AXIS2_PLACEMENT_3D('',#37658,#23165,#23166);
#19482=AXIS2_PLACEMENT_3D('',#37659,#23167,#23168);
#19483=AXIS2_PLACEMENT_3D('',#37665,#23172,#23173);
#19484=AXIS2_PLACEMENT_3D('',#37668,#23176,#23177);
#19485=AXIS2_PLACEMENT_3D('',#37674,#23181,#23182);
#19486=AXIS2_PLACEMENT_3D('',#37678,#23184,#23185);
#19487=AXIS2_PLACEMENT_3D('',#37686,#23189,#23190);
#19488=AXIS2_PLACEMENT_3D('',#37688,#23192,#23193);
#19489=AXIS2_PLACEMENT_3D('',#37693,#23195,#23196);
#19490=AXIS2_PLACEMENT_3D('',#37696,#23198,#23199);
#19491=AXIS2_PLACEMENT_3D('',#37697,#23200,#23201);
#19492=AXIS2_PLACEMENT_3D('',#37703,#23205,#23206);
#19493=AXIS2_PLACEMENT_3D('',#37706,#23209,#23210);
#19494=AXIS2_PLACEMENT_3D('',#37711,#23212,#23213);
#19495=AXIS2_PLACEMENT_3D('',#37714,#23215,#23216);
#19496=AXIS2_PLACEMENT_3D('',#37715,#23217,#23218);
#19497=AXIS2_PLACEMENT_3D('',#37720,#23222,#23223);
#19498=AXIS2_PLACEMENT_3D('',#37724,#23226,#23227);
#19499=AXIS2_PLACEMENT_3D('',#37728,#23229,#23230);
#19500=AXIS2_PLACEMENT_3D('',#37736,#23234,#23235);
#19501=AXIS2_PLACEMENT_3D('',#37738,#23237,#23238);
#19502=AXIS2_PLACEMENT_3D('',#37751,#23245,#23246);
#19503=AXIS2_PLACEMENT_3D('',#37760,#23251,#23252);
#19504=AXIS2_PLACEMENT_3D('',#37761,#23253,#23254);
#19505=AXIS2_PLACEMENT_3D('',#37770,#23259,#23260);
#19506=AXIS2_PLACEMENT_3D('',#37771,#23261,#23262);
#19507=AXIS2_PLACEMENT_3D('',#37775,#23264,#23265);
#19508=AXIS2_PLACEMENT_3D('',#37777,#23267,#23268);
#19509=AXIS2_PLACEMENT_3D('',#37783,#23272,#23273);
#19510=AXIS2_PLACEMENT_3D('',#37786,#23275,#23276);
#19511=AXIS2_PLACEMENT_3D('',#37787,#23277,#23278);
#19512=AXIS2_PLACEMENT_3D('',#37791,#23281,#23282);
#19513=AXIS2_PLACEMENT_3D('',#37795,#23285,#23286);
#19514=AXIS2_PLACEMENT_3D('',#37799,#23289,#23290);
#19515=AXIS2_PLACEMENT_3D('',#37802,#23292,#23293);
#19516=AXIS2_PLACEMENT_3D('',#37803,#23294,#23295);
#19517=AXIS2_PLACEMENT_3D('',#37809,#23299,#23300);
#19518=AXIS2_PLACEMENT_3D('',#37816,#23304,#23305);
#19519=AXIS2_PLACEMENT_3D('',#37817,#23306,#23307);
#19520=AXIS2_PLACEMENT_3D('',#37821,#23309,#23310);
#19521=AXIS2_PLACEMENT_3D('',#37823,#23312,#23313);
#19522=AXIS2_PLACEMENT_3D('',#37829,#23317,#23318);
#19523=AXIS2_PLACEMENT_3D('',#37832,#23320,#23321);
#19524=AXIS2_PLACEMENT_3D('',#37833,#23322,#23323);
#19525=AXIS2_PLACEMENT_3D('',#37837,#23326,#23327);
#19526=AXIS2_PLACEMENT_3D('',#37841,#23330,#23331);
#19527=AXIS2_PLACEMENT_3D('',#37845,#23334,#23335);
#19528=AXIS2_PLACEMENT_3D('',#37848,#23337,#23338);
#19529=AXIS2_PLACEMENT_3D('',#37849,#23339,#23340);
#19530=AXIS2_PLACEMENT_3D('',#37855,#23344,#23345);
#19531=AXIS2_PLACEMENT_3D('',#37862,#23349,#23350);
#19532=AXIS2_PLACEMENT_3D('',#37863,#23351,#23352);
#19533=AXIS2_PLACEMENT_3D('',#37867,#23354,#23355);
#19534=AXIS2_PLACEMENT_3D('',#37869,#23357,#23358);
#19535=AXIS2_PLACEMENT_3D('',#37875,#23362,#23363);
#19536=AXIS2_PLACEMENT_3D('',#37878,#23365,#23366);
#19537=AXIS2_PLACEMENT_3D('',#37879,#23367,#23368);
#19538=AXIS2_PLACEMENT_3D('',#37883,#23371,#23372);
#19539=AXIS2_PLACEMENT_3D('',#37887,#23375,#23376);
#19540=AXIS2_PLACEMENT_3D('',#37891,#23379,#23380);
#19541=AXIS2_PLACEMENT_3D('',#37894,#23382,#23383);
#19542=AXIS2_PLACEMENT_3D('',#37895,#23384,#23385);
#19543=AXIS2_PLACEMENT_3D('',#37901,#23389,#23390);
#19544=AXIS2_PLACEMENT_3D('',#37908,#23394,#23395);
#19545=AXIS2_PLACEMENT_3D('',#37909,#23396,#23397);
#19546=AXIS2_PLACEMENT_3D('',#37913,#23399,#23400);
#19547=AXIS2_PLACEMENT_3D('',#37915,#23402,#23403);
#19548=AXIS2_PLACEMENT_3D('',#37921,#23407,#23408);
#19549=AXIS2_PLACEMENT_3D('',#37924,#23410,#23411);
#19550=AXIS2_PLACEMENT_3D('',#37925,#23412,#23413);
#19551=AXIS2_PLACEMENT_3D('',#37929,#23416,#23417);
#19552=AXIS2_PLACEMENT_3D('',#37933,#23420,#23421);
#19553=AXIS2_PLACEMENT_3D('',#37937,#23424,#23425);
#19554=AXIS2_PLACEMENT_3D('',#37940,#23427,#23428);
#19555=AXIS2_PLACEMENT_3D('',#37941,#23429,#23430);
#19556=AXIS2_PLACEMENT_3D('',#37945,#23433,#23434);
#19557=AXIS2_PLACEMENT_3D('',#37951,#23438,#23439);
#19558=AXIS2_PLACEMENT_3D('',#37955,#23442,#23443);
#19559=AXIS2_PLACEMENT_3D('',#37959,#23446,#23447);
#19560=AXIS2_PLACEMENT_3D('',#37963,#23450,#23451);
#19561=AXIS2_PLACEMENT_3D('',#37967,#23454,#23455);
#19562=AXIS2_PLACEMENT_3D('',#37969,#23457,#23458);
#19563=AXIS2_PLACEMENT_3D('',#37970,#23459,#23460);
#19564=AXIS2_PLACEMENT_3D('',#37971,#23461,#23462);
#19565=AXIS2_PLACEMENT_3D('',#37974,#23465,#23466);
#19566=AXIS2_PLACEMENT_3D('',#37976,#23468,#23469);
#19567=AXIS2_PLACEMENT_3D('',#37978,#23471,#23472);
#19568=AXIS2_PLACEMENT_3D('',#37979,#23473,#23474);
#19569=AXIS2_PLACEMENT_3D('',#37980,#23475,#23476);
#19570=AXIS2_PLACEMENT_3D('',#37981,#23477,#23478);
#19571=AXIS2_PLACEMENT_3D('',#37982,#23479,#23480);
#19572=AXIS2_PLACEMENT_3D('',#37983,#23481,#23482);
#19573=AXIS2_PLACEMENT_3D('',#37989,#23486,#23487);
#19574=AXIS2_PLACEMENT_3D('',#37994,#23489,#23490);
#19575=AXIS2_PLACEMENT_3D('',#37997,#23492,#23493);
#19576=AXIS2_PLACEMENT_3D('',#38000,#23495,#23496);
#19577=AXIS2_PLACEMENT_3D('',#38001,#23497,#23498);
#19578=AXIS2_PLACEMENT_3D('',#38005,#23501,#23502);
#19579=AXIS2_PLACEMENT_3D('',#38008,#23504,#23505);
#19580=AXIS2_PLACEMENT_3D('',#38009,#23506,#23507);
#19581=AXIS2_PLACEMENT_3D('',#38013,#23510,#23511);
#19582=AXIS2_PLACEMENT_3D('',#38017,#23513,#23514);
#19583=AXIS2_PLACEMENT_3D('',#38020,#23516,#23517);
#19584=AXIS2_PLACEMENT_3D('',#38022,#23519,#23520);
#19585=AXIS2_PLACEMENT_3D('',#38024,#23522,#23523);
#19586=AXIS2_PLACEMENT_3D('',#38026,#23525,#23526);
#19587=AXIS2_PLACEMENT_3D('',#38028,#23528,#23529);
#19588=AXIS2_PLACEMENT_3D('',#38032,#23531,#23532);
#19589=AXIS2_PLACEMENT_3D('',#38036,#23534,#23535);
#19590=AXIS2_PLACEMENT_3D('',#38038,#23537,#23538);
#19591=AXIS2_PLACEMENT_3D('',#38042,#23541,#23542);
#19592=AXIS2_PLACEMENT_3D('',#38045,#23544,#23545);
#19593=AXIS2_PLACEMENT_3D('',#38046,#23546,#23547);
#19594=AXIS2_PLACEMENT_3D('',#38050,#23550,#23551);
#19595=AXIS2_PLACEMENT_3D('',#38054,#23553,#23554);
#19596=AXIS2_PLACEMENT_3D('',#38058,#23556,#23557);
#19597=AXIS2_PLACEMENT_3D('',#38061,#23559,#23560);
#19598=AXIS2_PLACEMENT_3D('',#38062,#23561,#23562);
#19599=AXIS2_PLACEMENT_3D('',#38066,#23565,#23566);
#19600=AXIS2_PLACEMENT_3D('',#38067,#23567,#23568);
#19601=AXIS2_PLACEMENT_3D('',#38068,#23569,#23570);
#19602=AXIS2_PLACEMENT_3D('',#38069,#23571,#23572);
#19603=AXIS2_PLACEMENT_3D('',#38082,#23579,#23580);
#19604=AXIS2_PLACEMENT_3D('',#38085,#23583,#23584);
#19605=AXIS2_PLACEMENT_3D('',#38087,#23586,#23587);
#19606=AXIS2_PLACEMENT_3D('',#38089,#23589,#23590);
#19607=AXIS2_PLACEMENT_3D('',#38091,#23592,#23593);
#19608=AXIS2_PLACEMENT_3D('',#38093,#23595,#23596);
#19609=AXIS2_PLACEMENT_3D('',#38095,#23598,#23599);
#19610=AXIS2_PLACEMENT_3D('',#38096,#23600,#23601);
#19611=AXIS2_PLACEMENT_3D('',#38098,#23603,#23604);
#19612=AXIS2_PLACEMENT_3D('',#38100,#23606,#23607);
#19613=AXIS2_PLACEMENT_3D('',#38102,#23609,#23610);
#19614=AXIS2_PLACEMENT_3D('',#38104,#23612,#23613);
#19615=AXIS2_PLACEMENT_3D('',#38106,#23615,#23616);
#19616=AXIS2_PLACEMENT_3D('',#38108,#23618,#23619);
#19617=AXIS2_PLACEMENT_3D('',#38110,#23621,#23622);
#19618=AXIS2_PLACEMENT_3D('',#38111,#23623,#23624);
#19619=AXIS2_PLACEMENT_3D('',#38128,#23633,#23634);
#19620=AXIS2_PLACEMENT_3D('',#38129,#23635,#23636);
#19621=AXIS2_PLACEMENT_3D('',#38130,#23637,#23638);
#19622=AXIS2_PLACEMENT_3D('',#38131,#23639,#23640);
#19623=AXIS2_PLACEMENT_3D('',#38133,#23641,#23642);
#19624=AXIS2_PLACEMENT_3D('',#38136,#23644,#23645);
#19625=AXIS2_PLACEMENT_3D('',#38137,#23646,#23647);
#19626=AXIS2_PLACEMENT_3D('',#38151,#23655,#23656);
#19627=AXIS2_PLACEMENT_3D('',#38164,#23663,#23664);
#19628=AXIS2_PLACEMENT_3D('',#38175,#23665,#23666);
#19629=AXIS2_PLACEMENT_3D('',#38181,#23670,#23671);
#19630=AXIS2_PLACEMENT_3D('',#38185,#23674,#23675);
#19631=AXIS2_PLACEMENT_3D('',#38189,#23678,#23679);
#19632=AXIS2_PLACEMENT_3D('',#38193,#23682,#23683);
#19633=AXIS2_PLACEMENT_3D('',#38197,#23686,#23687);
#19634=AXIS2_PLACEMENT_3D('',#38199,#23689,#23690);
#19635=AXIS2_PLACEMENT_3D('',#38203,#23692,#23693);
#19636=AXIS2_PLACEMENT_3D('',#38205,#23695,#23696);
#19637=AXIS2_PLACEMENT_3D('',#38206,#23697,#23698);
#19638=AXIS2_PLACEMENT_3D('',#38207,#23699,#23700);
#19639=AXIS2_PLACEMENT_3D('',#38208,#23701,#23702);
#19640=AXIS2_PLACEMENT_3D('',#38209,#23703,#23704);
#19641=AXIS2_PLACEMENT_3D('',#38210,#23705,#23706);
#19642=AXIS2_PLACEMENT_3D('',#38211,#23707,#23708);
#19643=AXIS2_PLACEMENT_3D('',#38212,#23709,#23710);
#19644=AXIS2_PLACEMENT_3D('',#38213,#23711,#23712);
#19645=AXIS2_PLACEMENT_3D('',#38216,#23713,#23714);
#19646=AXIS2_PLACEMENT_3D('',#38217,#23715,#23716);
#19647=AXIS2_PLACEMENT_3D('',#38218,#23717,#23718);
#19648=AXIS2_PLACEMENT_3D('',#38221,#23721,#23722);
#19649=AXIS2_PLACEMENT_3D('',#38234,#23729,#23730);
#19650=AXIS2_PLACEMENT_3D('',#38247,#23737,#23738);
#19651=AXIS2_PLACEMENT_3D('',#38260,#23745,#23746);
#19652=AXIS2_PLACEMENT_3D('',#38262,#23747,#23748);
#19653=AXIS2_PLACEMENT_3D('',#38264,#23750,#23751);
#19654=AXIS2_PLACEMENT_3D('',#38268,#23754,#23755);
#19655=AXIS2_PLACEMENT_3D('',#38269,#23756,#23757);
#19656=AXIS2_PLACEMENT_3D('',#38270,#23758,#23759);
#19657=AXIS2_PLACEMENT_3D('',#38272,#23760,#23761);
#19658=AXIS2_PLACEMENT_3D('',#38274,#23763,#23764);
#19659=AXIS2_PLACEMENT_3D('',#38278,#23767,#23768);
#19660=AXIS2_PLACEMENT_3D('',#38279,#23769,#23770);
#19661=AXIS2_PLACEMENT_3D('',#38280,#23771,#23772);
#19662=AXIS2_PLACEMENT_3D('',#38281,#23773,#23774);
#19663=AXIS2_PLACEMENT_3D('',#38282,#23775,#23776);
#19664=AXIS2_PLACEMENT_3D('',#38283,#23777,#23778);
#19665=AXIS2_PLACEMENT_3D('',#38285,#23779,#23780);
#19666=AXIS2_PLACEMENT_3D('',#38287,#23782,#23783);
#19667=AXIS2_PLACEMENT_3D('',#38291,#23786,#23787);
#19668=AXIS2_PLACEMENT_3D('',#38292,#23788,#23789);
#19669=AXIS2_PLACEMENT_3D('',#38293,#23790,#23791);
#19670=AXIS2_PLACEMENT_3D('',#38295,#23792,#23793);
#19671=AXIS2_PLACEMENT_3D('',#38297,#23795,#23796);
#19672=AXIS2_PLACEMENT_3D('',#38301,#23799,#23800);
#19673=AXIS2_PLACEMENT_3D('',#38302,#23801,#23802);
#19674=AXIS2_PLACEMENT_3D('',#38303,#23803,#23804);
#19675=AXIS2_PLACEMENT_3D('',#38309,#23808,#23809);
#19676=AXIS2_PLACEMENT_3D('',#38313,#23812,#23813);
#19677=AXIS2_PLACEMENT_3D('',#38317,#23816,#23817);
#19678=AXIS2_PLACEMENT_3D('',#38321,#23820,#23821);
#19679=AXIS2_PLACEMENT_3D('',#38325,#23824,#23825);
#19680=AXIS2_PLACEMENT_3D('',#38327,#23827,#23828);
#19681=AXIS2_PLACEMENT_3D('',#38329,#23829,#23830);
#19682=AXIS2_PLACEMENT_3D('',#38333,#23833,#23834);
#19683=AXIS2_PLACEMENT_3D('',#38335,#23835,#23836);
#19684=AXIS2_PLACEMENT_3D('',#38342,#23837,#23838);
#19685=AXIS2_PLACEMENT_3D('',#38346,#23840,#23841);
#19686=AXIS2_PLACEMENT_3D('',#38348,#23843,#23844);
#19687=AXIS2_PLACEMENT_3D('',#38357,#23846,#23847);
#19688=AXIS2_PLACEMENT_3D('',#38359,#23848,#23849);
#19689=AXIS2_PLACEMENT_3D('',#38360,#23850,#23851);
#19690=AXIS2_PLACEMENT_3D('',#38361,#23852,#23853);
#19691=AXIS2_PLACEMENT_3D('',#38374,#23860,#23861);
#19692=AXIS2_PLACEMENT_3D('',#38387,#23868,#23869);
#19693=AXIS2_PLACEMENT_3D('',#38400,#23876,#23877);
#19694=AXIS2_PLACEMENT_3D('',#38404,#23880,#23881);
#19695=AXIS2_PLACEMENT_3D('',#38408,#23884,#23885);
#19696=AXIS2_PLACEMENT_3D('',#38410,#23887,#23888);
#19697=AXIS2_PLACEMENT_3D('',#38423,#23895,#23896);
#19698=AXIS2_PLACEMENT_3D('',#38436,#23903,#23904);
#19699=AXIS2_PLACEMENT_3D('',#38442,#23908,#23909);
#19700=AXIS2_PLACEMENT_3D('',#38446,#23912,#23913);
#19701=AXIS2_PLACEMENT_3D('',#38450,#23916,#23917);
#19702=AXIS2_PLACEMENT_3D('',#38454,#23920,#23921);
#19703=AXIS2_PLACEMENT_3D('',#38458,#23924,#23925);
#19704=AXIS2_PLACEMENT_3D('',#38460,#23927,#23928);
#19705=AXIS2_PLACEMENT_3D('',#38465,#23930,#23931);
#19706=AXIS2_PLACEMENT_3D('',#38467,#23933,#23934);
#19707=AXIS2_PLACEMENT_3D('',#38471,#23936,#23937);
#19708=AXIS2_PLACEMENT_3D('',#38472,#23938,#23939);
#19709=AXIS2_PLACEMENT_3D('',#38473,#23940,#23941);
#19710=AXIS2_PLACEMENT_3D('',#38479,#23944,#23945);
#19711=AXIS2_PLACEMENT_3D('',#38481,#23947,#23948);
#19712=AXIS2_PLACEMENT_3D('',#38487,#23952,#23953);
#19713=AXIS2_PLACEMENT_3D('',#38491,#23956,#23957);
#19714=AXIS2_PLACEMENT_3D('',#38495,#23960,#23961);
#19715=AXIS2_PLACEMENT_3D('',#38499,#23964,#23965);
#19716=AXIS2_PLACEMENT_3D('',#38503,#23968,#23969);
#19717=AXIS2_PLACEMENT_3D('',#38505,#23971,#23972);
#19718=AXIS2_PLACEMENT_3D('',#38510,#23974,#23975);
#19719=AXIS2_PLACEMENT_3D('',#38513,#23977,#23978);
#19720=AXIS2_PLACEMENT_3D('',#38514,#23979,#23980);
#19721=AXIS2_PLACEMENT_3D('',#38518,#23982,#23983);
#19722=AXIS2_PLACEMENT_3D('',#38522,#23986,#23987);
#19723=AXIS2_PLACEMENT_3D('',#38528,#23991,#23992);
#19724=AXIS2_PLACEMENT_3D('',#38532,#23995,#23996);
#19725=AXIS2_PLACEMENT_3D('',#38536,#23999,#24000);
#19726=AXIS2_PLACEMENT_3D('',#38540,#24003,#24004);
#19727=AXIS2_PLACEMENT_3D('',#38544,#24007,#24008);
#19728=AXIS2_PLACEMENT_3D('',#38546,#24010,#24011);
#19729=AXIS2_PLACEMENT_3D('',#38562,#24013,#24014);
#19730=AXIS2_PLACEMENT_3D('',#38589,#24015,#24016);
#19731=AXIS2_PLACEMENT_3D('',#38602,#24017,#24018);
#19732=AXIS2_PLACEMENT_3D('',#38614,#24019,#24020);
#19733=AXIS2_PLACEMENT_3D('',#38618,#24022,#24023);
#19734=AXIS2_PLACEMENT_3D('',#38620,#24025,#24026);
#19735=AXIS2_PLACEMENT_3D('',#38622,#24027,#24028);
#19736=AXIS2_PLACEMENT_3D('',#38629,#24029,#24030);
#19737=AXIS2_PLACEMENT_3D('',#38632,#24031,#24032);
#19738=AXIS2_PLACEMENT_3D('',#38635,#24035,#24036);
#19739=AXIS2_PLACEMENT_3D('',#38644,#24038,#24039);
#19740=AXIS2_PLACEMENT_3D('',#38645,#24040,#24041);
#19741=AXIS2_PLACEMENT_3D('',#38646,#24042,#24043);
#19742=AXIS2_PLACEMENT_3D('',#38673,#24044,#24045);
#19743=AXIS2_PLACEMENT_3D('',#38700,#24046,#24047);
#19744=AXIS2_PLACEMENT_3D('',#38716,#24049,#24050);
#19745=AXIS2_PLACEMENT_3D('',#38720,#24054,#24055);
#19746=AXIS2_PLACEMENT_3D('',#38723,#24057,#24058);
#19747=AXIS2_PLACEMENT_3D('',#38843,#24059,#24060);
#19748=AXIS2_PLACEMENT_3D('',#38852,#24064,#24065);
#19749=AXIS2_PLACEMENT_3D('',#38856,#24068,#24069);
#19750=AXIS2_PLACEMENT_3D('',#38857,#24070,#24071);
#19751=AXIS2_PLACEMENT_3D('',#38861,#24073,#24074);
#19752=AXIS2_PLACEMENT_3D('',#38863,#24076,#24077);
#19753=AXIS2_PLACEMENT_3D('',#38866,#24079,#24080);
#19754=AXIS2_PLACEMENT_3D('',#38867,#24081,#24082);
#19755=AXIS2_PLACEMENT_3D('',#38869,#24083,#24084);
#19756=AXIS2_PLACEMENT_3D('',#38873,#24087,#24088);
#19757=AXIS2_PLACEMENT_3D('',#38877,#24090,#24091);
#19758=AXIS2_PLACEMENT_3D('',#38880,#24094,#24095);
#19759=AXIS2_PLACEMENT_3D('',#38886,#24099,#24100);
#19760=AXIS2_PLACEMENT_3D('',#38890,#24103,#24104);
#19761=AXIS2_PLACEMENT_3D('',#38894,#24107,#24108);
#19762=AXIS2_PLACEMENT_3D('',#38898,#24111,#24112);
#19763=AXIS2_PLACEMENT_3D('',#38902,#24115,#24116);
#19764=AXIS2_PLACEMENT_3D('',#38978,#24118,#24119);
#19765=AXIS2_PLACEMENT_3D('',#38982,#24121,#24122);
#19766=AXIS2_PLACEMENT_3D('',#38984,#24124,#24125);
#19767=AXIS2_PLACEMENT_3D('',#38987,#24127,#24128);
#19768=AXIS2_PLACEMENT_3D('',#38988,#24129,#24130);
#19769=AXIS2_PLACEMENT_3D('',#38993,#24133,#24134);
#19770=AXIS2_PLACEMENT_3D('',#38994,#24135,#24136);
#19771=AXIS2_PLACEMENT_3D('',#39000,#24140,#24141);
#19772=AXIS2_PLACEMENT_3D('',#39004,#24144,#24145);
#19773=AXIS2_PLACEMENT_3D('',#39008,#24148,#24149);
#19774=AXIS2_PLACEMENT_3D('',#39012,#24152,#24153);
#19775=AXIS2_PLACEMENT_3D('',#39016,#24156,#24157);
#19776=AXIS2_PLACEMENT_3D('',#39018,#24159,#24160);
#19777=AXIS2_PLACEMENT_3D('',#39024,#24164,#24165);
#19778=AXIS2_PLACEMENT_3D('',#39028,#24168,#24169);
#19779=AXIS2_PLACEMENT_3D('',#39032,#24172,#24173);
#19780=AXIS2_PLACEMENT_3D('',#39036,#24176,#24177);
#19781=AXIS2_PLACEMENT_3D('',#39040,#24180,#24181);
#19782=AXIS2_PLACEMENT_3D('',#39042,#24183,#24184);
#19783=AXIS2_PLACEMENT_3D('',#39043,#24185,#24186);
#19784=AXIS2_PLACEMENT_3D('',#39056,#24193,#24194);
#19785=AXIS2_PLACEMENT_3D('',#39057,#24195,#24196);
#19786=AXIS2_PLACEMENT_3D('',#39070,#24203,#24204);
#19787=AXIS2_PLACEMENT_3D('',#39076,#24208,#24209);
#19788=AXIS2_PLACEMENT_3D('',#39086,#24215,#24216);
#19789=AXIS2_PLACEMENT_3D('',#39092,#24220,#24221);
#19790=AXIS2_PLACEMENT_3D('',#39098,#24225,#24226);
#19791=AXIS2_PLACEMENT_3D('',#39102,#24229,#24230);
#19792=AXIS2_PLACEMENT_3D('',#39106,#24233,#24234);
#19793=AXIS2_PLACEMENT_3D('',#39110,#24237,#24238);
#19794=AXIS2_PLACEMENT_3D('',#39114,#24241,#24242);
#19795=AXIS2_PLACEMENT_3D('',#39116,#24244,#24245);
#19796=AXIS2_PLACEMENT_3D('',#39119,#24246,#24247);
#19797=AXIS2_PLACEMENT_3D('',#39126,#24252,#24253);
#19798=AXIS2_PLACEMENT_3D('',#39130,#24256,#24257);
#19799=AXIS2_PLACEMENT_3D('',#39134,#24260,#24261);
#19800=AXIS2_PLACEMENT_3D('',#39140,#24264,#24265);
#19801=AXIS2_PLACEMENT_3D('',#39142,#24267,#24268);
#19802=AXIS2_PLACEMENT_3D('',#39146,#24271,#24272);
#19803=AXIS2_PLACEMENT_3D('',#39148,#24274,#24275);
#19804=AXIS2_PLACEMENT_3D('',#39149,#24276,#24277);
#19805=AXIS2_PLACEMENT_3D('',#39151,#24279,#24280);
#19806=AXIS2_PLACEMENT_3D('',#39153,#24281,#24282);
#19807=AXIS2_PLACEMENT_3D('',#39231,#24284,#24285);
#19808=AXIS2_PLACEMENT_3D('',#39232,#24286,#24287);
#19809=AXIS2_PLACEMENT_3D('',#39236,#24290,#24291);
#19810=AXIS2_PLACEMENT_3D('',#39237,#24292,#24293);
#19811=AXIS2_PLACEMENT_3D('',#39241,#24295,#24296);
#19812=AXIS2_PLACEMENT_3D('',#39317,#24298,#24299);
#19813=AXIS2_PLACEMENT_3D('',#39323,#24303,#24304);
#19814=AXIS2_PLACEMENT_3D('',#39326,#24305,#24306);
#19815=AXIS2_PLACEMENT_3D('',#39329,#24309,#24310);
#19816=AXIS2_PLACEMENT_3D('',#39333,#24313,#24314);
#19817=AXIS2_PLACEMENT_3D('',#39335,#24316,#24317);
#19818=AXIS2_PLACEMENT_3D('',#39338,#24319,#24320);
#19819=AXIS2_PLACEMENT_3D('',#39339,#24321,#24322);
#19820=AXIS2_PLACEMENT_3D('',#39341,#24323,#24324);
#19821=AXIS2_PLACEMENT_3D('',#39343,#24326,#24327);
#19822=AXIS2_PLACEMENT_3D('',#39345,#24328,#24329);
#19823=AXIS2_PLACEMENT_3D('',#39347,#24331,#24332);
#19824=AXIS2_PLACEMENT_3D('',#39348,#24333,#24334);
#19825=AXIS2_PLACEMENT_3D('',#39354,#24338,#24339);
#19826=AXIS2_PLACEMENT_3D('',#39358,#24342,#24343);
#19827=AXIS2_PLACEMENT_3D('',#39362,#24346,#24347);
#19828=AXIS2_PLACEMENT_3D('',#39366,#24350,#24351);
#19829=AXIS2_PLACEMENT_3D('',#39370,#24354,#24355);
#19830=AXIS2_PLACEMENT_3D('',#39372,#24357,#24358);
#19831=AXIS2_PLACEMENT_3D('',#39374,#24360,#24361);
#19832=AXIS2_PLACEMENT_3D('',#39376,#24363,#24364);
#19833=AXIS2_PLACEMENT_3D('',#39382,#24368,#24369);
#19834=AXIS2_PLACEMENT_3D('',#39386,#24372,#24373);
#19835=AXIS2_PLACEMENT_3D('',#39390,#24376,#24377);
#19836=AXIS2_PLACEMENT_3D('',#39392,#24379,#24380);
#19837=AXIS2_PLACEMENT_3D('',#39394,#24382,#24383);
#19838=AXIS2_PLACEMENT_3D('',#39395,#24384,#24385);
#19839=AXIS2_PLACEMENT_3D('',#39397,#24387,#24388);
#19840=AXIS2_PLACEMENT_3D('',#39400,#24391,#24392);
#19841=AXIS2_PLACEMENT_3D('',#39404,#24394,#24395);
#19842=AXIS2_PLACEMENT_3D('',#39405,#24396,#24397);
#19843=AXIS2_PLACEMENT_3D('',#39409,#24399,#24400);
#19844=AXIS2_PLACEMENT_3D('',#39410,#24401,#24402);
#19845=AXIS2_PLACEMENT_3D('',#39412,#24404,#24405);
#19846=AXIS2_PLACEMENT_3D('',#39416,#24408,#24409);
#19847=AXIS2_PLACEMENT_3D('',#39419,#24410,#24411);
#19848=AXIS2_PLACEMENT_3D('',#39421,#24413,#24414);
#19849=AXIS2_PLACEMENT_3D('',#39422,#24415,#24416);
#19850=AXIS2_PLACEMENT_3D('',#39426,#24419,#24420);
#19851=AXIS2_PLACEMENT_3D('',#39429,#24421,#24422);
#19852=AXIS2_PLACEMENT_3D('',#39431,#24424,#24425);
#19853=AXIS2_PLACEMENT_3D('',#39432,#24426,#24427);
#19854=AXIS2_PLACEMENT_3D('',#39435,#24430,#24431);
#19855=AXIS2_PLACEMENT_3D('',#39437,#24433,#24434);
#19856=AXIS2_PLACEMENT_3D('',#39441,#24436,#24437);
#19857=AXIS2_PLACEMENT_3D('',#39442,#24438,#24439);
#19858=AXIS2_PLACEMENT_3D('',#39446,#24441,#24442);
#19859=AXIS2_PLACEMENT_3D('',#39447,#24443,#24444);
#19860=AXIS2_PLACEMENT_3D('',#39449,#24445,#24446);
#19861=AXIS2_PLACEMENT_3D('',#39450,#24447,#24448);
#19862=AXIS2_PLACEMENT_3D('',#39451,#24449,#24450);
#19863=AXIS2_PLACEMENT_3D('',#39453,#24451,#24452);
#19864=AXIS2_PLACEMENT_3D('',#39455,#24453,#24454);
#19865=AXIS2_PLACEMENT_3D('',#39464,#24455,#24456);
#19866=AXIS2_PLACEMENT_3D('',#39466,#24457,#24458);
#19867=AXIS2_PLACEMENT_3D('',#39468,#24459,#24460);
#19868=AXIS2_PLACEMENT_3D('',#39470,#24461,#24462);
#19869=AXIS2_PLACEMENT_3D('',#39472,#24463,#24464);
#19870=AXIS2_PLACEMENT_3D('',#39473,#24465,#24466);
#19871=AXIS2_PLACEMENT_3D('',#39474,#24467,#24468);
#19872=AXIS2_PLACEMENT_3D('',#39483,#24469,#24470);
#19873=AXIS2_PLACEMENT_3D('',#39484,#24471,#24472);
#19874=AXIS2_PLACEMENT_3D('',#39485,#24473,#24474);
#19875=AXIS2_PLACEMENT_3D('',#39486,#24475,#24476);
#19876=AXIS2_PLACEMENT_3D('',#39498,#24483,#24484);
#19877=AXIS2_PLACEMENT_3D('',#39502,#24487,#24488);
#19878=AXIS2_PLACEMENT_3D('',#39508,#24492,#24493);
#19879=AXIS2_PLACEMENT_3D('',#39512,#24496,#24497);
#19880=AXIS2_PLACEMENT_3D('',#39518,#24501,#24502);
#19881=AXIS2_PLACEMENT_3D('',#39522,#24505,#24506);
#19882=AXIS2_PLACEMENT_3D('',#39542,#24517,#24518);
#19883=AXIS2_PLACEMENT_3D('',#39546,#24521,#24522);
#19884=AXIS2_PLACEMENT_3D('',#39552,#24526,#24527);
#19885=AXIS2_PLACEMENT_3D('',#39556,#24530,#24531);
#19886=AXIS2_PLACEMENT_3D('',#39562,#24535,#24536);
#19887=AXIS2_PLACEMENT_3D('',#39566,#24539,#24540);
#19888=AXIS2_PLACEMENT_3D('',#39576,#24546,#24547);
#19889=AXIS2_PLACEMENT_3D('',#39582,#24551,#24552);
#19890=AXIS2_PLACEMENT_3D('',#39584,#24553,#24554);
#19891=AXIS2_PLACEMENT_3D('',#39587,#24557,#24558);
#19892=AXIS2_PLACEMENT_3D('',#39590,#24559,#24560);
#19893=AXIS2_PLACEMENT_3D('',#39593,#24563,#24564);
#19894=AXIS2_PLACEMENT_3D('',#39596,#24565,#24566);
#19895=AXIS2_PLACEMENT_3D('',#39599,#24569,#24570);
#19896=AXIS2_PLACEMENT_3D('',#39608,#24577,#24578);
#19897=AXIS2_PLACEMENT_3D('',#39612,#24581,#24582);
#19898=AXIS2_PLACEMENT_3D('',#39614,#24584,#24585);
#19899=AXIS2_PLACEMENT_3D('',#39616,#24587,#24588);
#19900=AXIS2_PLACEMENT_3D('',#39620,#24591,#24592);
#19901=AXIS2_PLACEMENT_3D('',#39624,#24595,#24596);
#19902=AXIS2_PLACEMENT_3D('',#39632,#24602,#24603);
#19903=AXIS2_PLACEMENT_3D('',#39633,#24604,#24605);
#19904=AXIS2_PLACEMENT_3D('',#39634,#24606,#24607);
#19905=AXIS2_PLACEMENT_3D('',#39640,#24608,#24609);
#19906=AXIS2_PLACEMENT_3D('',#39641,#24610,#24611);
#19907=AXIS2_PLACEMENT_3D('',#39643,#24612,#24613);
#19908=AXIS2_PLACEMENT_3D('',#39648,#24614,#24615);
#19909=AXIS2_PLACEMENT_3D('',#39654,#24616,#24617);
#19910=AXIS2_PLACEMENT_3D('',#39655,#24618,#24619);
#19911=AXIS2_PLACEMENT_3D('',#39656,#24620,#24621);
#19912=AXIS2_PLACEMENT_3D('',#39657,#24622,#24623);
#19913=AXIS2_PLACEMENT_3D('',#39665,#24628,#24629);
#19914=AXIS2_PLACEMENT_3D('',#39671,#24633,#24634);
#19915=AXIS2_PLACEMENT_3D('',#39675,#24637,#24638);
#19916=AXIS2_PLACEMENT_3D('',#39677,#24640,#24641);
#19917=AXIS2_PLACEMENT_3D('',#39679,#24643,#24644);
#19918=AXIS2_PLACEMENT_3D('',#39682,#24647,#24648);
#19919=AXIS2_PLACEMENT_3D('',#39688,#24652,#24653);
#19920=AXIS2_PLACEMENT_3D('',#39692,#24656,#24657);
#19921=AXIS2_PLACEMENT_3D('',#39696,#24660,#24661);
#19922=AXIS2_PLACEMENT_3D('',#39702,#24665,#24666);
#19923=AXIS2_PLACEMENT_3D('',#39708,#24670,#24671);
#19924=AXIS2_PLACEMENT_3D('',#39712,#24674,#24675);
#19925=AXIS2_PLACEMENT_3D('',#39716,#24678,#24679);
#19926=AXIS2_PLACEMENT_3D('',#39718,#24681,#24682);
#19927=AXIS2_PLACEMENT_3D('',#39720,#24684,#24685);
#19928=AXIS2_PLACEMENT_3D('',#39722,#24687,#24688);
#19929=AXIS2_PLACEMENT_3D('',#39730,#24693,#24694);
#19930=AXIS2_PLACEMENT_3D('',#39734,#24697,#24698);
#19931=AXIS2_PLACEMENT_3D('',#39740,#24702,#24703);
#19932=AXIS2_PLACEMENT_3D('',#39746,#24707,#24708);
#19933=AXIS2_PLACEMENT_3D('',#39750,#24711,#24712);
#19934=AXIS2_PLACEMENT_3D('',#39754,#24715,#24716);
#19935=AXIS2_PLACEMENT_3D('',#39758,#24719,#24720);
#19936=AXIS2_PLACEMENT_3D('',#39762,#24723,#24724);
#19937=AXIS2_PLACEMENT_3D('',#39766,#24727,#24728);
#19938=AXIS2_PLACEMENT_3D('',#39770,#24731,#24732);
#19939=AXIS2_PLACEMENT_3D('',#39774,#24735,#24736);
#19940=AXIS2_PLACEMENT_3D('',#39778,#24739,#24740);
#19941=AXIS2_PLACEMENT_3D('',#39782,#24743,#24744);
#19942=AXIS2_PLACEMENT_3D('',#39786,#24747,#24748);
#19943=AXIS2_PLACEMENT_3D('',#39788,#24750,#24751);
#19944=AXIS2_PLACEMENT_3D('',#39789,#24752,#24753);
#19945=AXIS2_PLACEMENT_3D('',#39790,#24754,#24755);
#19946=AXIS2_PLACEMENT_3D('',#39793,#24756,#24757);
#19947=AXIS2_PLACEMENT_3D('',#39794,#24758,#24759);
#19948=AXIS2_PLACEMENT_3D('',#39796,#24760,#24761);
#19949=AXIS2_PLACEMENT_3D('',#39797,#24762,#24763);
#19950=AXIS2_PLACEMENT_3D('',#39798,#24764,#24765);
#19951=AXIS2_PLACEMENT_3D('',#39801,#24766,#24767);
#19952=AXIS2_PLACEMENT_3D('',#39803,#24768,#24769);
#19953=AXIS2_PLACEMENT_3D('',#39805,#24770,#24771);
#19954=AXIS2_PLACEMENT_3D('',#39808,#24773,#24774);
#19955=AXIS2_PLACEMENT_3D('',#39810,#24775,#24776);
#19956=AXIS2_PLACEMENT_3D('',#39812,#24777,#24778);
#19957=AXIS2_PLACEMENT_3D('',#39813,#24779,#24780);
#19958=AXIS2_PLACEMENT_3D('',#39814,#24781,#24782);
#19959=AXIS2_PLACEMENT_3D('',#39816,#24783,#24784);
#19960=AXIS2_PLACEMENT_3D('',#39819,#24786,#24787);
#19961=AXIS2_PLACEMENT_3D('',#39820,#24788,#24789);
#19962=AXIS2_PLACEMENT_3D('',#39822,#24791,#24792);
#19963=AXIS2_PLACEMENT_3D('',#39823,#24793,#24794);
#19964=AXIS2_PLACEMENT_3D('',#39824,#24795,#24796);
#19965=AXIS2_PLACEMENT_3D('',#39828,#24799,#24800);
#19966=AXIS2_PLACEMENT_3D('',#39832,#24803,#24804);
#19967=AXIS2_PLACEMENT_3D('',#39836,#24807,#24808);
#19968=AXIS2_PLACEMENT_3D('',#39840,#24811,#24812);
#19969=AXIS2_PLACEMENT_3D('',#39844,#24815,#24816);
#19970=AXIS2_PLACEMENT_3D('',#39848,#24819,#24820);
#19971=AXIS2_PLACEMENT_3D('',#39851,#24821,#24822);
#19972=AXIS2_PLACEMENT_3D('',#39853,#24823,#24824);
#19973=AXIS2_PLACEMENT_3D('',#39855,#24825,#24826);
#19974=AXIS2_PLACEMENT_3D('',#39857,#24827,#24828);
#19975=AXIS2_PLACEMENT_3D('',#39859,#24829,#24830);
#19976=AXIS2_PLACEMENT_3D('',#39860,#24831,#24832);
#19977=AXIS2_PLACEMENT_3D('',#39861,#24833,#24834);
#19978=AXIS2_PLACEMENT_3D('',#39869,#24835,#24836);
#19979=AXIS2_PLACEMENT_3D('',#39877,#24837,#24838);
#19980=AXIS2_PLACEMENT_3D('',#39885,#24839,#24840);
#19981=AXIS2_PLACEMENT_3D('',#39893,#24841,#24842);
#19982=AXIS2_PLACEMENT_3D('',#39901,#24843,#24844);
#19983=AXIS2_PLACEMENT_3D('',#39909,#24845,#24846);
#19984=AXIS2_PLACEMENT_3D('',#39912,#24849,#24850);
#19985=AXIS2_PLACEMENT_3D('',#39914,#24852,#24853);
#19986=AXIS2_PLACEMENT_3D('',#39916,#24855,#24856);
#19987=AXIS2_PLACEMENT_3D('',#39918,#24858,#24859);
#19988=AXIS2_PLACEMENT_3D('',#39920,#24861,#24862);
#19989=AXIS2_PLACEMENT_3D('',#39921,#24863,#24864);
#19990=AXIS2_PLACEMENT_3D('',#39922,#24865,#24866);
#19991=AXIS2_PLACEMENT_3D('',#39923,#24867,#24868);
#19992=AXIS2_PLACEMENT_3D('',#39924,#24869,#24870);
#19993=AXIS2_PLACEMENT_3D('',#39925,#24871,#24872);
#19994=AXIS2_PLACEMENT_3D('',#39926,#24873,#24874);
#19995=AXIS2_PLACEMENT_3D('',#39927,#24875,#24876);
#19996=AXIS2_PLACEMENT_3D('',#39928,#24877,#24878);
#19997=AXIS2_PLACEMENT_3D('',#39929,#24879,#24880);
#19998=AXIS2_PLACEMENT_3D('',#39930,#24881,#24882);
#19999=AXIS2_PLACEMENT_3D('',#39931,#24883,#24884);
#20000=AXIS2_PLACEMENT_3D('',#39932,#24885,#24886);
#20001=AXIS2_PLACEMENT_3D('',#39933,#24887,#24888);
#20002=AXIS2_PLACEMENT_3D('',#39934,#24889,#24890);
#20003=AXIS2_PLACEMENT_3D('',#39935,#24891,#24892);
#20004=AXIS2_PLACEMENT_3D('',#39936,#24893,#24894);
#20005=AXIS2_PLACEMENT_3D('',#39937,#24895,#24896);
#20006=AXIS2_PLACEMENT_3D('',#39938,#24897,#24898);
#20007=AXIS2_PLACEMENT_3D('',#39939,#24899,#24900);
#20008=AXIS2_PLACEMENT_3D('',#39940,#24901,#24902);
#20009=AXIS2_PLACEMENT_3D('',#39941,#24903,#24904);
#20010=DIRECTION('axis',(0.,0.,1.));
#20011=DIRECTION('refdir',(1.,0.,0.));
#20012=DIRECTION('axis',(0.,0.,1.));
#20013=DIRECTION('refdir',(1.,0.,0.));
#20014=DIRECTION('center_axis',(0.,0.,1.));
#20015=DIRECTION('ref_axis',(1.,0.,0.));
#20016=DIRECTION('center_axis',(0.,0.,1.));
#20017=DIRECTION('ref_axis',(1.,0.,0.));
#20018=DIRECTION('center_axis',(1.22464679914735E-16,-1.,0.));
#20019=DIRECTION('ref_axis',(-1.,-1.22464679914735E-16,0.));
#20020=DIRECTION('center_axis',(0.,0.,-1.));
#20021=DIRECTION('ref_axis',(1.,0.,0.));
#20022=DIRECTION('center_axis',(0.,0.,1.));
#20023=DIRECTION('ref_axis',(1.,0.,0.));
#20024=DIRECTION('center_axis',(0.,0.,1.));
#20025=DIRECTION('ref_axis',(1.,0.,0.));
#20026=DIRECTION('center_axis',(0.,0.,1.));
#20027=DIRECTION('ref_axis',(1.,0.,0.));
#20028=DIRECTION('center_axis',(1.22464679914735E-16,-1.,0.));
#20029=DIRECTION('ref_axis',(-1.,-1.22464679914735E-16,0.));
#20030=DIRECTION('center_axis',(0.,0.,-1.));
#20031=DIRECTION('ref_axis',(1.,0.,0.));
#20032=DIRECTION('center_axis',(0.,0.,-1.));
#20033=DIRECTION('ref_axis',(-1.,0.,0.));
#20034=DIRECTION('center_axis',(0.,0.,1.));
#20035=DIRECTION('ref_axis',(1.,0.,0.));
#20036=DIRECTION('',(0.,0.,1.));
#20037=DIRECTION('center_axis',(0.255411479413649,0.147461886393592,-0.955520783784934));
#20038=DIRECTION('ref_axis',(-0.827505272601769,-0.47776039189247,-0.294923772787182));
#20039=DIRECTION('',(0.,0.,1.));
#20040=DIRECTION('center_axis',(0.,0.,1.));
#20041=DIRECTION('ref_axis',(1.,0.,0.));
#20042=DIRECTION('',(0.,0.,1.));
#20043=DIRECTION('center_axis',(0.100869871038817,0.277137692982455,-0.955520783784934));
#20044=DIRECTION('ref_axis',(-0.326807355420773,-0.897895829530272,-0.294923772787182));
#20045=DIRECTION('',(0.,0.,1.));
#20046=DIRECTION('center_axis',(0.,0.,1.));
#20047=DIRECTION('ref_axis',(1.,0.,0.));
#20048=DIRECTION('',(0.,0.,1.));
#20049=DIRECTION('center_axis',(-0.100869871038821,0.277137692982454,-0.955520783784934));
#20050=DIRECTION('ref_axis',(-0.326807355420785,0.897895829530268,0.294923772787182));
#20051=DIRECTION('',(0.,0.,1.));
#20052=DIRECTION('center_axis',(0.,0.,1.));
#20053=DIRECTION('ref_axis',(1.,0.,0.));
#20054=DIRECTION('',(0.,0.,1.));
#20055=DIRECTION('center_axis',(-0.255411479413651,0.147461886393589,-0.955520783784934));
#20056=DIRECTION('ref_axis',(-0.827505272601775,0.47776039189246,0.294923772787182));
#20057=DIRECTION('',(0.,0.,1.));
#20058=DIRECTION('center_axis',(0.,0.,1.));
#20059=DIRECTION('ref_axis',(1.,0.,0.));
#20060=DIRECTION('',(0.,0.,1.));
#20061=DIRECTION('center_axis',(0.,0.,1.));
#20062=DIRECTION('ref_axis',(1.,0.,0.));
#20063=DIRECTION('center_axis',(0.,0.,1.));
#20064=DIRECTION('ref_axis',(1.,0.,0.));
#20065=DIRECTION('',(0.,0.,1.));
#20066=DIRECTION('center_axis',(-0.290443217988427,-0.0512129756951529,
-0.955520783784934));
#20067=DIRECTION('ref_axis',(-0.941004276035703,-0.165924442827141,0.294923772787182));
#20068=DIRECTION('',(0.,0.,1.));
#20069=DIRECTION('center_axis',(0.,0.,1.));
#20070=DIRECTION('ref_axis',(1.,0.,0.));
#20071=DIRECTION('',(0.,0.,1.));
#20072=DIRECTION('center_axis',(-0.189573346949606,-0.225924717287307,-0.955520783784934));
#20073=DIRECTION('ref_axis',(-0.614196920614917,-0.731971386703147,0.294923772787182));
#20074=DIRECTION('',(0.,0.,1.));
#20075=DIRECTION('center_axis',(0.,0.,1.));
#20076=DIRECTION('ref_axis',(1.,0.,0.));
#20077=DIRECTION('',(0.,0.,1.));
#20078=DIRECTION('center_axis',(0.,-0.294923772787182,-0.955520783784934));
#20079=DIRECTION('ref_axis',(0.,0.955520783784934,-0.294923772787182));
#20080=DIRECTION('',(0.,0.,1.));
#20081=DIRECTION('center_axis',(0.,0.,1.));
#20082=DIRECTION('ref_axis',(1.,0.,0.));
#20083=DIRECTION('',(0.,0.,1.));
#20084=DIRECTION('center_axis',(0.189573346949609,-0.225924717287304,-0.955520783784934));
#20085=DIRECTION('ref_axis',(-0.614196920614927,0.731971386703139,-0.294923772787182));
#20086=DIRECTION('',(0.,0.,1.));
#20087=DIRECTION('center_axis',(0.,0.,1.));
#20088=DIRECTION('ref_axis',(1.,0.,0.));
#20089=DIRECTION('',(0.,0.,1.));
#20090=DIRECTION('center_axis',(0.290443217988428,-0.0512129756951491,-0.955520783784934));
#20091=DIRECTION('ref_axis',(-0.941004276035705,0.165924442827128,-0.294923772787182));
#20092=DIRECTION('',(0.,0.,1.));
#20093=DIRECTION('center_axis',(-1.,-1.26189474349424E-16,0.));
#20094=DIRECTION('ref_axis',(1.26189474349424E-16,-1.,0.));
#20095=DIRECTION('center_axis',(1.,1.26189474349424E-16,0.));
#20096=DIRECTION('ref_axis',(1.26189474349424E-16,-1.,0.));
#20097=DIRECTION('',(-1.,-1.26189474349424E-16,0.));
#20098=DIRECTION('center_axis',(1.,1.26189474349424E-16,0.));
#20099=DIRECTION('ref_axis',(1.26189474349424E-16,-1.,0.));
#20100=DIRECTION('center_axis',(-1.,-1.26189474349424E-16,0.));
#20101=DIRECTION('ref_axis',(1.26189474349424E-16,-1.,0.));
#20102=DIRECTION('center_axis',(1.,1.26189474349424E-16,0.));
#20103=DIRECTION('ref_axis',(-1.26189474349424E-16,1.,0.));
#20104=DIRECTION('',(-1.,-1.26189474349424E-16,0.));
#20105=DIRECTION('center_axis',(1.,1.26189474349424E-16,0.));
#20106=DIRECTION('ref_axis',(-1.26189474349424E-16,1.,0.));
#20107=DIRECTION('center_axis',(-1.,-1.26189474349424E-16,0.));
#20108=DIRECTION('ref_axis',(1.26189474349424E-16,-1.,0.));
#20109=DIRECTION('center_axis',(1.,1.26189474349424E-16,0.));
#20110=DIRECTION('ref_axis',(1.26189474349424E-16,-1.,0.));
#20111=DIRECTION('',(-1.,-1.26189474349424E-16,0.));
#20112=DIRECTION('center_axis',(1.,1.26189474349424E-16,0.));
#20113=DIRECTION('ref_axis',(1.26189474349424E-16,-1.,0.));
#20114=DIRECTION('center_axis',(-1.,-1.26189474349424E-16,0.));
#20115=DIRECTION('ref_axis',(1.26189474349424E-16,-1.,0.));
#20116=DIRECTION('center_axis',(1.,1.26189474349424E-16,0.));
#20117=DIRECTION('ref_axis',(-1.26189474349424E-16,1.,0.));
#20118=DIRECTION('',(-1.,-1.26189474349424E-16,0.));
#20119=DIRECTION('center_axis',(1.,1.26189474349424E-16,0.));
#20120=DIRECTION('ref_axis',(-1.26189474349424E-16,1.,0.));
#20121=DIRECTION('center_axis',(-1.,-1.26189474349424E-16,0.));
#20122=DIRECTION('ref_axis',(1.26189474349424E-16,-1.,0.));
#20123=DIRECTION('center_axis',(1.,1.26189474349424E-16,0.));
#20124=DIRECTION('ref_axis',(1.26189474349424E-16,-1.,0.));
#20125=DIRECTION('',(-1.,-1.26189474349424E-16,0.));
#20126=DIRECTION('center_axis',(1.,1.26189474349424E-16,0.));
#20127=DIRECTION('ref_axis',(1.26189474349424E-16,-1.,0.));
#20128=DIRECTION('center_axis',(-1.,-1.26189474349424E-16,0.));
#20129=DIRECTION('ref_axis',(1.26189474349424E-16,-1.,0.));
#20130=DIRECTION('center_axis',(1.,1.26189474349424E-16,0.));
#20131=DIRECTION('ref_axis',(1.26189474349424E-16,-1.,0.));
#20132=DIRECTION('',(-1.,-1.26189474349424E-16,0.));
#20133=DIRECTION('center_axis',(1.,1.26189474349424E-16,0.));
#20134=DIRECTION('ref_axis',(1.26189474349424E-16,-1.,0.));
#20135=DIRECTION('center_axis',(-1.,-1.26189474349424E-16,0.));
#20136=DIRECTION('ref_axis',(1.26189474349424E-16,-1.,0.));
#20137=DIRECTION('center_axis',(1.,1.26189474349424E-16,0.));
#20138=DIRECTION('ref_axis',(-1.26189474349424E-16,1.,0.));
#20139=DIRECTION('',(-1.,-1.26189474349424E-16,0.));
#20140=DIRECTION('center_axis',(1.,1.26189474349424E-16,0.));
#20141=DIRECTION('ref_axis',(-1.26189474349424E-16,1.,0.));
#20142=DIRECTION('center_axis',(-1.,-1.26189474349424E-16,0.));
#20143=DIRECTION('ref_axis',(1.26189474349424E-16,-1.,0.));
#20144=DIRECTION('center_axis',(1.,1.26189474349424E-16,0.));
#20145=DIRECTION('ref_axis',(-1.26189474349424E-16,1.,0.));
#20146=DIRECTION('',(-1.,-1.26189474349424E-16,0.));
#20147=DIRECTION('center_axis',(1.,1.26189474349424E-16,0.));
#20148=DIRECTION('ref_axis',(-1.26189474349424E-16,1.,0.));
#20149=DIRECTION('center_axis',(-1.,-1.26189474349424E-16,0.));
#20150=DIRECTION('ref_axis',(1.26189474349424E-16,-1.,0.));
#20151=DIRECTION('',(1.,1.26189474349424E-16,0.));
#20152=DIRECTION('center_axis',(-1.,-1.26189474349424E-16,0.));
#20153=DIRECTION('ref_axis',(1.26189474349424E-16,-1.,0.));
#20154=DIRECTION('center_axis',(-1.,-1.26189474349424E-16,0.));
#20155=DIRECTION('ref_axis',(1.26189474349424E-16,-1.,0.));
#20156=DIRECTION('',(1.,1.26189474349424E-16,0.));
#20157=DIRECTION('center_axis',(-1.,-1.26189474349424E-16,0.));
#20158=DIRECTION('ref_axis',(-1.26189474349424E-16,1.,0.));
#20159=DIRECTION('center_axis',(1.,-3.84524791680814E-16,0.));
#20160=DIRECTION('ref_axis',(-3.84524791680814E-16,-1.,0.));
#20161=DIRECTION('',(1.,-3.84524791680814E-16,0.));
#20162=DIRECTION('center_axis',(1.,1.26189474349424E-16,0.));
#20163=DIRECTION('ref_axis',(1.26189474349424E-16,-1.,0.));
#20164=DIRECTION('center_axis',(1.,3.84524791680814E-16,0.));
#20165=DIRECTION('ref_axis',(-3.84524791680814E-16,1.,0.));
#20166=DIRECTION('',(1.,3.84524791680814E-16,0.));
#20167=DIRECTION('center_axis',(1.,1.26189474349424E-16,0.));
#20168=DIRECTION('ref_axis',(-1.26189474349424E-16,1.,0.));
#20169=DIRECTION('center_axis',(0.,0.,1.));
#20170=DIRECTION('ref_axis',(1.,0.,0.));
#20171=DIRECTION('',(0.,0.,1.));
#20172=DIRECTION('center_axis',(0.,0.,1.));
#20173=DIRECTION('ref_axis',(1.,0.,0.));
#20174=DIRECTION('center_axis',(0.,0.,1.));
#20175=DIRECTION('ref_axis',(1.,0.,0.));
#20176=DIRECTION('center_axis',(0.,0.,1.));
#20177=DIRECTION('ref_axis',(1.,0.,0.));
#20178=DIRECTION('',(0.,0.,1.));
#20179=DIRECTION('center_axis',(0.,0.,1.));
#20180=DIRECTION('ref_axis',(1.,0.,0.));
#20181=DIRECTION('center_axis',(0.,0.,1.));
#20182=DIRECTION('ref_axis',(1.,0.,0.));
#20183=DIRECTION('center_axis',(0.,0.,1.));
#20184=DIRECTION('ref_axis',(1.,0.,0.));
#20185=DIRECTION('',(0.,0.,1.));
#20186=DIRECTION('center_axis',(0.,0.,1.));
#20187=DIRECTION('ref_axis',(1.,0.,0.));
#20188=DIRECTION('center_axis',(0.,0.,1.));
#20189=DIRECTION('ref_axis',(1.,0.,0.));
#20190=DIRECTION('center_axis',(0.,0.,1.));
#20191=DIRECTION('ref_axis',(1.,0.,0.));
#20192=DIRECTION('',(0.,0.,1.));
#20193=DIRECTION('center_axis',(0.,0.,1.));
#20194=DIRECTION('ref_axis',(1.,0.,0.));
#20195=DIRECTION('center_axis',(0.,0.,1.));
#20196=DIRECTION('ref_axis',(1.,0.,0.));
#20197=DIRECTION('center_axis',(0.,0.,1.));
#20198=DIRECTION('ref_axis',(1.,0.,0.));
#20199=DIRECTION('',(0.,0.,1.));
#20200=DIRECTION('center_axis',(0.,0.,1.));
#20201=DIRECTION('ref_axis',(1.,0.,0.));
#20202=DIRECTION('center_axis',(0.,0.,1.));
#20203=DIRECTION('ref_axis',(1.,0.,0.));
#20204=DIRECTION('center_axis',(0.,0.,1.));
#20205=DIRECTION('ref_axis',(1.,0.,0.));
#20206=DIRECTION('',(0.,0.,1.));
#20207=DIRECTION('center_axis',(0.,0.,1.));
#20208=DIRECTION('ref_axis',(1.,0.,0.));
#20209=DIRECTION('center_axis',(0.,0.,1.));
#20210=DIRECTION('ref_axis',(1.,0.,0.));
#20211=DIRECTION('center_axis',(0.,0.,1.));
#20212=DIRECTION('ref_axis',(1.,0.,0.));
#20213=DIRECTION('',(0.,0.,1.));
#20214=DIRECTION('center_axis',(0.,0.,1.));
#20215=DIRECTION('ref_axis',(1.,0.,0.));
#20216=DIRECTION('center_axis',(0.,0.,1.));
#20217=DIRECTION('ref_axis',(1.,0.,0.));
#20218=DIRECTION('center_axis',(0.,0.,1.));
#20219=DIRECTION('ref_axis',(1.,0.,0.));
#20220=DIRECTION('',(0.,0.,1.));
#20221=DIRECTION('center_axis',(0.,0.,1.));
#20222=DIRECTION('ref_axis',(1.,0.,0.));
#20223=DIRECTION('center_axis',(0.,0.,1.));
#20224=DIRECTION('ref_axis',(1.,0.,0.));
#20225=DIRECTION('center_axis',(0.,0.,1.));
#20226=DIRECTION('ref_axis',(1.,0.,0.));
#20227=DIRECTION('',(0.,0.,1.));
#20228=DIRECTION('center_axis',(0.,0.,1.));
#20229=DIRECTION('ref_axis',(1.,0.,0.));
#20230=DIRECTION('center_axis',(0.,0.,1.));
#20231=DIRECTION('ref_axis',(1.,0.,0.));
#20232=DIRECTION('center_axis',(0.,0.,1.));
#20233=DIRECTION('ref_axis',(1.,0.,0.));
#20234=DIRECTION('',(0.,0.,1.));
#20235=DIRECTION('center_axis',(0.,0.,1.));
#20236=DIRECTION('ref_axis',(1.,0.,0.));
#20237=DIRECTION('center_axis',(0.,0.,1.));
#20238=DIRECTION('ref_axis',(1.,0.,0.));
#20239=DIRECTION('center_axis',(0.,0.,1.));
#20240=DIRECTION('ref_axis',(1.,0.,0.));
#20241=DIRECTION('',(0.,0.,1.));
#20242=DIRECTION('center_axis',(0.,0.,1.));
#20243=DIRECTION('ref_axis',(1.,0.,0.));
#20244=DIRECTION('center_axis',(0.,0.,1.));
#20245=DIRECTION('ref_axis',(1.,0.,0.));
#20246=DIRECTION('center_axis',(0.,0.,1.));
#20247=DIRECTION('ref_axis',(1.,0.,0.));
#20248=DIRECTION('',(0.,0.,1.));
#20249=DIRECTION('center_axis',(0.,0.,1.));
#20250=DIRECTION('ref_axis',(1.,0.,0.));
#20251=DIRECTION('center_axis',(0.,0.,1.));
#20252=DIRECTION('ref_axis',(1.,0.,0.));
#20253=DIRECTION('center_axis',(0.,0.,1.));
#20254=DIRECTION('ref_axis',(1.,0.,0.));
#20255=DIRECTION('',(0.,0.,1.));
#20256=DIRECTION('center_axis',(0.,0.,1.));
#20257=DIRECTION('ref_axis',(1.,0.,0.));
#20258=DIRECTION('center_axis',(0.,0.,1.));
#20259=DIRECTION('ref_axis',(1.,0.,0.));
#20260=DIRECTION('center_axis',(0.,0.,1.));
#20261=DIRECTION('ref_axis',(1.,0.,0.));
#20262=DIRECTION('',(0.,0.,1.));
#20263=DIRECTION('center_axis',(0.,0.,1.));
#20264=DIRECTION('ref_axis',(1.,0.,0.));
#20265=DIRECTION('center_axis',(0.,0.,1.));
#20266=DIRECTION('ref_axis',(1.,0.,0.));
#20267=DIRECTION('center_axis',(0.,0.,1.));
#20268=DIRECTION('ref_axis',(1.,0.,0.));
#20269=DIRECTION('',(0.,0.,1.));
#20270=DIRECTION('center_axis',(0.,0.,1.));
#20271=DIRECTION('ref_axis',(1.,0.,0.));
#20272=DIRECTION('center_axis',(0.,0.,1.));
#20273=DIRECTION('ref_axis',(1.,0.,0.));
#20274=DIRECTION('center_axis',(0.,0.,1.));
#20275=DIRECTION('ref_axis',(1.,0.,0.));
#20276=DIRECTION('',(0.,0.,1.));
#20277=DIRECTION('center_axis',(0.,0.,1.));
#20278=DIRECTION('ref_axis',(1.,0.,0.));
#20279=DIRECTION('center_axis',(0.,0.,-1.));
#20280=DIRECTION('ref_axis',(-1.,0.,0.));
#20281=DIRECTION('',(0.,0.,1.));
#20282=DIRECTION('center_axis',(0.,0.,1.));
#20283=DIRECTION('ref_axis',(1.,0.,0.));
#20284=DIRECTION('center_axis',(0.,0.,1.));
#20285=DIRECTION('ref_axis',(1.,0.,0.));
#20286=DIRECTION('center_axis',(0.,0.,1.));
#20287=DIRECTION('ref_axis',(1.,0.,0.));
#20288=DIRECTION('',(0.,0.,-1.));
#20289=DIRECTION('center_axis',(0.,0.,1.));
#20290=DIRECTION('ref_axis',(1.,0.,0.));
#20291=DIRECTION('center_axis',(0.,0.,1.));
#20292=DIRECTION('ref_axis',(1.,0.,0.));
#20293=DIRECTION('center_axis',(0.,0.,-1.));
#20294=DIRECTION('ref_axis',(1.,0.,0.));
#20295=DIRECTION('',(0.,0.,1.));
#20296=DIRECTION('center_axis',(0.,0.,1.));
#20297=DIRECTION('ref_axis',(1.,0.,0.));
#20298=DIRECTION('center_axis',(0.,0.,1.));
#20299=DIRECTION('ref_axis',(1.,0.,0.));
#20300=DIRECTION('',(0.64278760968653,0.766044443118986,0.));
#20301=DIRECTION('',(0.984807753012206,0.17364817766694,0.));
#20302=DIRECTION('',(-0.17364817766694,0.984807753012206,0.));
#20303=DIRECTION('',(0.984807753012206,0.17364817766694,0.));
#20304=DIRECTION('',(0.866025403784443,-0.499999999999992,0.));
#20305=DIRECTION('',(0.499999999999992,0.866025403784443,0.));
#20306=DIRECTION('',(0.866025403784443,-0.499999999999992,0.));
#20307=DIRECTION('',(0.342020143325676,-0.939692620785906,0.));
#20308=DIRECTION('',(0.939692620785906,0.342020143325676,0.));
#20309=DIRECTION('',(0.342020143325676,-0.939692620785906,0.));
#20310=DIRECTION('',(-0.342020143325663,-0.93969262078591,0.));
#20311=DIRECTION('',(0.93969262078591,-0.342020143325663,0.));
#20312=DIRECTION('',(-0.342020143325663,-0.93969262078591,0.));
#20313=DIRECTION('',(-0.866025403784436,-0.500000000000004,0.));
#20314=DIRECTION('',(0.500000000000004,-0.866025403784436,0.));
#20315=DIRECTION('',(-0.866025403784436,-0.500000000000004,0.));
#20316=DIRECTION('',(-0.984807753012209,0.173648177666927,0.));
#20317=DIRECTION('',(-0.173648177666927,-0.984807753012209,0.));
#20318=DIRECTION('',(-0.984807753012209,0.173648177666927,0.));
#20319=DIRECTION('',(-0.64278760968654,0.766044443118977,0.));
#20320=DIRECTION('',(-0.766044443118977,-0.64278760968654,0.));
#20321=DIRECTION('',(-0.64278760968654,0.766044443118977,0.));
#20322=DIRECTION('',(0.,1.,0.));
#20323=DIRECTION('',(-1.,0.,0.));
#20324=DIRECTION('',(0.,1.,0.));
#20325=DIRECTION('',(0.64278760968653,0.766044443118986,0.));
#20326=DIRECTION('',(-0.766044443118986,0.64278760968653,0.));
#20327=DIRECTION('center_axis',(0.,0.,1.));
#20328=DIRECTION('ref_axis',(1.,0.,0.));
#20329=DIRECTION('center_axis',(0.,0.,1.));
#20330=DIRECTION('ref_axis',(1.,0.,0.));
#20331=DIRECTION('center_axis',(0.,0.,1.));
#20332=DIRECTION('ref_axis',(1.,0.,0.));
#20333=DIRECTION('center_axis',(1.,1.26189474349424E-16,0.));
#20334=DIRECTION('ref_axis',(-1.26189474349424E-16,1.,0.));
#20335=DIRECTION('center_axis',(1.,1.26189474349424E-16,0.));
#20336=DIRECTION('ref_axis',(-1.26189474349424E-16,1.,0.));
#20337=DIRECTION('',(-1.38777878078145E-15,1.,0.));
#20338=DIRECTION('center_axis',(1.,1.26189474349424E-16,0.));
#20339=DIRECTION('ref_axis',(1.26189474349424E-16,-1.,0.));
#20340=DIRECTION('',(0.,0.,1.));
#20341=DIRECTION('center_axis',(1.,1.26189474349424E-16,0.));
#20342=DIRECTION('ref_axis',(1.26189474349424E-16,-1.,0.));
#20343=DIRECTION('',(1.38777878078145E-15,-1.,0.));
#20344=DIRECTION('center_axis',(1.,1.26189474349424E-16,0.));
#20345=DIRECTION('ref_axis',(1.26189474349424E-16,-1.,0.));
#20346=DIRECTION('',(0.,0.,-1.));
#20347=DIRECTION('center_axis',(1.,1.26189474349424E-16,0.));
#20348=DIRECTION('ref_axis',(-1.26189474349424E-16,1.,0.));
#20349=DIRECTION('center_axis',(1.,1.26189474349424E-16,0.));
#20350=DIRECTION('ref_axis',(-1.26189474349424E-16,1.,0.));
#20351=DIRECTION('',(0.,0.,-1.));
#20352=DIRECTION('center_axis',(1.,1.26189474349424E-16,0.));
#20353=DIRECTION('ref_axis',(1.26189474349424E-16,-1.,0.));
#20354=DIRECTION('',(1.38777878078145E-15,-1.,0.));
#20355=DIRECTION('center_axis',(1.,1.26189474349424E-16,0.));
#20356=DIRECTION('ref_axis',(1.26189474349424E-16,-1.,0.));
#20357=DIRECTION('',(0.,0.,1.));
#20358=DIRECTION('center_axis',(1.,1.26189474349424E-16,0.));
#20359=DIRECTION('ref_axis',(1.26189474349424E-16,-1.,0.));
#20360=DIRECTION('',(-1.38777878078145E-15,1.,0.));
#20361=DIRECTION('center_axis',(-1.,-1.26189474349424E-16,0.));
#20362=DIRECTION('ref_axis',(1.26189474349424E-16,-1.,0.));
#20363=DIRECTION('',(-1.,-1.26189474349424E-16,0.));
#20364=DIRECTION('',(-1.,-1.26189474349424E-16,0.));
#20365=DIRECTION('center_axis',(0.,0.,1.));
#20366=DIRECTION('ref_axis',(1.,0.,0.));
#20367=DIRECTION('',(-1.,-1.26189474349424E-16,0.));
#20368=DIRECTION('center_axis',(-1.,-1.26189474349424E-16,0.));
#20369=DIRECTION('ref_axis',(1.26189474349424E-16,-1.,0.));
#20370=DIRECTION('',(-1.,-1.26189474349424E-16,0.));
#20371=DIRECTION('center_axis',(1.26189474349424E-16,-1.,0.));
#20372=DIRECTION('ref_axis',(1.,1.26189474349424E-16,0.));
#20373=DIRECTION('',(-1.,-1.26189474349424E-16,0.));
#20374=DIRECTION('center_axis',(-1.,-1.26189474349424E-16,0.));
#20375=DIRECTION('ref_axis',(1.26189474349424E-16,-1.,0.));
#20376=DIRECTION('',(-1.,-1.26189474349424E-16,0.));
#20377=DIRECTION('center_axis',(0.,0.,-1.));
#20378=DIRECTION('ref_axis',(-1.,0.,0.));
#20379=DIRECTION('',(-1.,-1.26189474349424E-16,0.));
#20380=DIRECTION('center_axis',(-1.,-1.26189474349424E-16,0.));
#20381=DIRECTION('ref_axis',(1.26189474349424E-16,-1.,0.));
#20382=DIRECTION('',(-1.,-1.26189474349424E-16,0.));
#20383=DIRECTION('center_axis',(-1.26189474349424E-16,1.,0.));
#20384=DIRECTION('ref_axis',(-1.,-1.26189474349424E-16,0.));
#20385=DIRECTION('center_axis',(1.,1.26189474349424E-16,0.));
#20386=DIRECTION('ref_axis',(-1.26189474349424E-16,1.,0.));
#20387=DIRECTION('center_axis',(1.,1.26189474349424E-16,0.));
#20388=DIRECTION('ref_axis',(-1.26189474349424E-16,1.,0.));
#20389=DIRECTION('',(-1.38777878078145E-15,1.,0.));
#20390=DIRECTION('center_axis',(1.,1.26189474349424E-16,0.));
#20391=DIRECTION('ref_axis',(1.26189474349424E-16,-1.,0.));
#20392=DIRECTION('',(0.,0.,1.));
#20393=DIRECTION('center_axis',(1.,1.26189474349424E-16,0.));
#20394=DIRECTION('ref_axis',(-1.26189474349424E-16,1.,0.));
#20395=DIRECTION('',(1.38777878078145E-15,-1.,0.));
#20396=DIRECTION('center_axis',(1.,1.26189474349424E-16,0.));
#20397=DIRECTION('ref_axis',(-1.26189474349424E-16,1.,0.));
#20398=DIRECTION('',(0.,0.,-1.));
#20399=DIRECTION('center_axis',(1.,1.26189474349424E-16,0.));
#20400=DIRECTION('ref_axis',(-1.26189474349424E-16,1.,0.));
#20401=DIRECTION('center_axis',(1.,1.26189474349424E-16,0.));
#20402=DIRECTION('ref_axis',(-1.26189474349424E-16,1.,0.));
#20403=DIRECTION('',(0.,0.,-1.));
#20404=DIRECTION('center_axis',(1.,1.26189474349424E-16,0.));
#20405=DIRECTION('ref_axis',(-1.26189474349424E-16,1.,0.));
#20406=DIRECTION('',(1.38777878078145E-15,-1.,0.));
#20407=DIRECTION('center_axis',(1.,1.26189474349424E-16,0.));
#20408=DIRECTION('ref_axis',(-1.26189474349424E-16,1.,0.));
#20409=DIRECTION('',(0.,0.,1.));
#20410=DIRECTION('center_axis',(1.,1.26189474349424E-16,0.));
#20411=DIRECTION('ref_axis',(1.26189474349424E-16,-1.,0.));
#20412=DIRECTION('',(-1.38777878078145E-15,1.,0.));
#20413=DIRECTION('center_axis',(-1.,-1.26189474349424E-16,0.));
#20414=DIRECTION('ref_axis',(1.26189474349424E-16,-1.,0.));
#20415=DIRECTION('',(-1.,-1.26189474349424E-16,0.));
#20416=DIRECTION('',(-1.,-1.26189474349424E-16,0.));
#20417=DIRECTION('center_axis',(0.,0.,1.));
#20418=DIRECTION('ref_axis',(1.,0.,0.));
#20419=DIRECTION('',(-1.,-1.26189474349424E-16,0.));
#20420=DIRECTION('center_axis',(-1.,-1.26189474349424E-16,0.));
#20421=DIRECTION('ref_axis',(1.26189474349424E-16,-1.,0.));
#20422=DIRECTION('',(-1.,-1.26189474349424E-16,0.));
#20423=DIRECTION('center_axis',(1.26189474349424E-16,-1.,0.));
#20424=DIRECTION('ref_axis',(1.,1.26189474349424E-16,0.));
#20425=DIRECTION('',(-1.,-1.26189474349424E-16,0.));
#20426=DIRECTION('center_axis',(-1.,-1.26189474349424E-16,0.));
#20427=DIRECTION('ref_axis',(1.26189474349424E-16,-1.,0.));
#20428=DIRECTION('',(-1.,-1.26189474349424E-16,0.));
#20429=DIRECTION('center_axis',(0.,0.,-1.));
#20430=DIRECTION('ref_axis',(-1.,0.,0.));
#20431=DIRECTION('',(-1.,-1.26189474349424E-16,0.));
#20432=DIRECTION('center_axis',(-1.,-1.26189474349424E-16,0.));
#20433=DIRECTION('ref_axis',(1.26189474349424E-16,-1.,0.));
#20434=DIRECTION('',(-1.,-1.26189474349424E-16,0.));
#20435=DIRECTION('center_axis',(-1.26189474349424E-16,1.,0.));
#20436=DIRECTION('ref_axis',(-1.,-1.26189474349424E-16,0.));
#20437=DIRECTION('center_axis',(0.,0.,1.));
#20438=DIRECTION('ref_axis',(1.,0.,0.));
#20439=DIRECTION('center_axis',(1.,0.,0.));
#20440=DIRECTION('ref_axis',(0.,0.,-1.));
#20441=DIRECTION('',(0.,-0.955520783784934,0.294923772787182));
#20442=DIRECTION('center_axis',(1.,0.,0.));
#20443=DIRECTION('ref_axis',(0.,0.,-1.));
#20444=DIRECTION('',(0.,-0.955520783784934,0.294923772787182));
#20445=DIRECTION('center_axis',(0.,-0.294923772787182,-0.955520783784934));
#20446=DIRECTION('ref_axis',(0.,0.955520783784934,-0.294923772787182));
#20447=DIRECTION('center_axis',(0.766044443118977,0.64278760968654,0.));
#20448=DIRECTION('ref_axis',(0.,0.,-1.));
#20449=DIRECTION('',(0.614196920614927,-0.731971386703138,0.294923772787182));
#20450=DIRECTION('center_axis',(0.766044443118977,0.64278760968654,0.));
#20451=DIRECTION('ref_axis',(0.,0.,-1.));
#20452=DIRECTION('',(0.614196920614927,-0.731971386703138,0.294923772787182));
#20453=DIRECTION('center_axis',(0.189573346949609,-0.225924717287304,-0.955520783784934));
#20454=DIRECTION('ref_axis',(5.1741255323139E-18,0.973167658917659,-0.230097169988514));
#20455=DIRECTION('center_axis',(0.173648177666927,0.984807753012209,0.));
#20456=DIRECTION('ref_axis',(0.,0.,-1.));
#20457=DIRECTION('',(0.941004276035705,-0.165924442827128,0.294923772787182));
#20458=DIRECTION('center_axis',(0.173648177666927,0.984807753012209,0.));
#20459=DIRECTION('ref_axis',(0.,0.,-1.));
#20460=DIRECTION('',(0.941004276035705,-0.165924442827128,0.294923772787182));
#20461=DIRECTION('center_axis',(0.290443217988428,-0.0512129756951491,-0.955520783784934));
#20462=DIRECTION('ref_axis',(-0.95677630912777,-2.49539129740611E-18,-0.290824851571943));
#20463=DIRECTION('center_axis',(-0.500000000000004,0.866025403784436,0.));
#20464=DIRECTION('ref_axis',(0.,0.,-1.));
#20465=DIRECTION('',(0.827505272601769,0.477760391892471,0.294923772787182));
#20466=DIRECTION('center_axis',(-0.500000000000004,0.866025403784436,0.));
#20467=DIRECTION('ref_axis',(0.,0.,-1.));
#20468=DIRECTION('',(0.827505272601769,0.477760391892471,0.294923772787182));
#20469=DIRECTION('center_axis',(0.255411479413649,0.147461886393592,-0.955520783784934));
#20470=DIRECTION('ref_axis',(-0.966082247190219,-2.695277852006E-19,-0.25823456713596));
#20471=DIRECTION('center_axis',(-0.939692620785911,0.342020143325663,0.));
#20472=DIRECTION('ref_axis',(0.,0.,-1.));
#20473=DIRECTION('',(0.326807355420773,0.897895829530272,0.294923772787182));
#20474=DIRECTION('center_axis',(-0.939692620785911,0.342020143325663,0.));
#20475=DIRECTION('ref_axis',(0.,0.,-1.));
#20476=DIRECTION('',(0.326807355420773,0.897895829530272,0.294923772787182));
#20477=DIRECTION('center_axis',(0.100869871038817,0.277137692982455,-0.955520783784934));
#20478=DIRECTION('ref_axis',(2.8977398537934E-18,0.960419279714667,0.278558444769426));
#20479=DIRECTION('center_axis',(-0.939692620785906,-0.342020143325676,0.));
#20480=DIRECTION('ref_axis',(0.,0.,-1.));
#20481=DIRECTION('',(-0.326807355420785,0.897895829530268,0.294923772787182));
#20482=DIRECTION('center_axis',(-0.939692620785906,-0.342020143325676,0.));
#20483=DIRECTION('ref_axis',(0.,0.,-1.));
#20484=DIRECTION('',(-0.326807355420785,0.897895829530268,0.294923772787182));
#20485=DIRECTION('center_axis',(-0.100869871038821,0.277137692982454,-0.955520783784934));
#20486=DIRECTION('ref_axis',(-1.67311827781928E-19,0.960419279714667,0.278558444769425));
#20487=DIRECTION('center_axis',(-0.499999999999992,-0.866025403784443,0.));
#20488=DIRECTION('ref_axis',(0.,0.,-1.));
#20489=DIRECTION('',(-0.827505272601775,0.477760391892459,0.294923772787182));
#20490=DIRECTION('center_axis',(-0.499999999999992,-0.866025403784443,0.));
#20491=DIRECTION('ref_axis',(0.,0.,-1.));
#20492=DIRECTION('',(-0.827505272601775,0.477760391892459,0.294923772787182));
#20493=DIRECTION('center_axis',(-0.255411479413651,0.147461886393589,-0.955520783784934));
#20494=DIRECTION('ref_axis',(-0.966082247190218,-1.82035480917452E-18,0.258234567135962));
#20495=DIRECTION('center_axis',(0.17364817766694,-0.984807753012206,0.));
#20496=DIRECTION('ref_axis',(0.,0.,-1.));
#20497=DIRECTION('',(-0.941004276035703,-0.16592444282714,0.294923772787182));
#20498=DIRECTION('center_axis',(0.17364817766694,-0.984807753012206,0.));
#20499=DIRECTION('ref_axis',(0.,0.,-1.));
#20500=DIRECTION('',(-0.941004276035703,-0.16592444282714,0.294923772787182));
#20501=DIRECTION('center_axis',(-0.290443217988427,-0.0512129756951529,
-0.955520783784934));
#20502=DIRECTION('ref_axis',(-0.95677630912777,-5.00082995194373E-19,0.290824851571942));
#20503=DIRECTION('center_axis',(0.766044443118986,-0.64278760968653,0.));
#20504=DIRECTION('ref_axis',(0.,0.,-1.));
#20505=DIRECTION('',(-0.614196920614917,-0.731971386703147,0.294923772787182));
#20506=DIRECTION('center_axis',(0.766044443118986,-0.64278760968653,0.));
#20507=DIRECTION('ref_axis',(0.,0.,-1.));
#20508=DIRECTION('',(-0.614196920614917,-0.731971386703147,0.294923772787182));
#20509=DIRECTION('center_axis',(-0.189573346949606,-0.225924717287307,-0.955520783784934));
#20510=DIRECTION('ref_axis',(4.39360789729016E-18,0.973167658917658,-0.230097169988516));
#20511=DIRECTION('axis',(0.,0.,1.));
#20512=DIRECTION('refdir',(1.,0.,0.));
#20513=DIRECTION('center_axis',(0.,0.,-1.));
#20514=DIRECTION('ref_axis',(-1.,0.,0.));
#20515=DIRECTION('center_axis',(0.,0.,-1.));
#20516=DIRECTION('ref_axis',(1.,0.,0.));
#20517=DIRECTION('',(0.,0.,-1.));
#20518=DIRECTION('center_axis',(0.,0.,-1.));
#20519=DIRECTION('ref_axis',(1.,0.,0.));
#20520=DIRECTION('',(0.,0.,-1.));
#20521=DIRECTION('center_axis',(0.,0.,-1.));
#20522=DIRECTION('ref_axis',(-1.,0.,0.));
#20523=DIRECTION('center_axis',(0.,0.,1.));
#20524=DIRECTION('ref_axis',(1.,0.,0.));
#20525=DIRECTION('center_axis',(0.,0.,1.));
#20526=DIRECTION('ref_axis',(1.,0.,0.));
#20527=DIRECTION('center_axis',(1.,0.,0.));
#20528=DIRECTION('ref_axis',(0.,0.,-1.));
#20529=DIRECTION('center_axis',(1.,0.,0.));
#20530=DIRECTION('ref_axis',(0.,0.,-1.));
#20531=DIRECTION('',(1.,0.,0.));
#20532=DIRECTION('center_axis',(0.,0.,-1.));
#20533=DIRECTION('ref_axis',(-1.,0.,0.));
#20534=DIRECTION('center_axis',(0.,0.,1.));
#20535=DIRECTION('ref_axis',(1.,0.,0.));
#20536=DIRECTION('',(0.,0.,1.));
#20537=DIRECTION('center_axis',(0.,0.,1.));
#20538=DIRECTION('ref_axis',(1.,0.,0.));
#20539=DIRECTION('',(0.,0.,-1.));
#20540=DIRECTION('center_axis',(0.,0.,1.));
#20541=DIRECTION('ref_axis',(1.,0.,0.));
#20542=DIRECTION('center_axis',(0.,0.,-1.));
#20543=DIRECTION('ref_axis',(-1.,0.,0.));
#20544=DIRECTION('center_axis',(0.,0.,1.));
#20545=DIRECTION('ref_axis',(1.,0.,0.));
#20546=DIRECTION('center_axis',(0.,0.,1.));
#20547=DIRECTION('ref_axis',(-1.,0.,0.));
#20548=DIRECTION('center_axis',(0.,0.,1.));
#20549=DIRECTION('ref_axis',(1.,0.,0.));
#20550=DIRECTION('center_axis',(0.,0.,-1.));
#20551=DIRECTION('ref_axis',(1.,0.,0.));
#20552=DIRECTION('center_axis',(1.,0.,0.));
#20553=DIRECTION('ref_axis',(0.,0.,-1.));
#20554=DIRECTION('center_axis',(0.,0.,1.));
#20555=DIRECTION('ref_axis',(-1.,1.22464679914735E-16,0.));
#20556=DIRECTION('',(0.,0.,1.));
#20557=DIRECTION('center_axis',(0.,0.,1.));
#20558=DIRECTION('ref_axis',(1.,0.,0.));
#20559=DIRECTION('',(0.,0.,1.));
#20560=DIRECTION('center_axis',(0.,0.,1.));
#20561=DIRECTION('ref_axis',(-1.,1.22464679914735E-16,0.));
#20562=DIRECTION('center_axis',(0.,0.,-1.));
#20563=DIRECTION('ref_axis',(1.,0.,0.));
#20564=DIRECTION('center_axis',(0.,0.,1.));
#20565=DIRECTION('ref_axis',(1.,0.,0.));
#20566=DIRECTION('center_axis',(0.,0.,-1.));
#20567=DIRECTION('ref_axis',(1.,0.,0.));
#20568=DIRECTION('center_axis',(0.,0.,-1.));
#20569=DIRECTION('ref_axis',(-1.,0.,0.));
#20570=DIRECTION('center_axis',(0.,0.,-1.));
#20571=DIRECTION('ref_axis',(-1.,0.,0.));
#20572=DIRECTION('center_axis',(0.,0.,-1.));
#20573=DIRECTION('ref_axis',(-1.,0.,0.));
#20574=DIRECTION('center_axis',(0.,0.,-1.));
#20575=DIRECTION('ref_axis',(-1.,0.,0.));
#20576=DIRECTION('center_axis',(0.,0.,-1.));
#20577=DIRECTION('ref_axis',(-1.,0.,0.));
#20578=DIRECTION('center_axis',(0.,0.,-1.));
#20579=DIRECTION('ref_axis',(-1.,0.,0.));
#20580=DIRECTION('center_axis',(0.,0.,-1.));
#20581=DIRECTION('ref_axis',(-1.,0.,0.));
#20582=DIRECTION('center_axis',(0.,0.,-1.));
#20583=DIRECTION('ref_axis',(-1.,0.,0.));
#20584=DIRECTION('center_axis',(0.,0.,1.));
#20585=DIRECTION('ref_axis',(1.,0.,0.));
#20586=DIRECTION('center_axis',(0.,0.,1.));
#20587=DIRECTION('ref_axis',(-1.,0.,0.));
#20588=DIRECTION('',(0.,0.,1.));
#20589=DIRECTION('center_axis',(0.,0.,1.));
#20590=DIRECTION('ref_axis',(-1.,0.,0.));
#20591=DIRECTION('',(0.,0.,1.));
#20592=DIRECTION('center_axis',(0.,0.,1.));
#20593=DIRECTION('ref_axis',(1.,0.,0.));
#20594=DIRECTION('center_axis',(0.,0.,-1.));
#20595=DIRECTION('ref_axis',(-1.,0.,0.));
#20596=DIRECTION('center_axis',(0.,0.,-1.));
#20597=DIRECTION('ref_axis',(-1.,0.,0.));
#20598=DIRECTION('center_axis',(-1.,0.,0.));
#20599=DIRECTION('ref_axis',(0.,0.,1.));
#20600=DIRECTION('center_axis',(-1.,0.,0.));
#20601=DIRECTION('ref_axis',(0.,0.,1.));
#20602=DIRECTION('',(-1.,0.,0.));
#20603=DIRECTION('center_axis',(0.,0.,1.));
#20604=DIRECTION('ref_axis',(1.,0.,0.));
#20605=DIRECTION('center_axis',(0.,0.,-1.));
#20606=DIRECTION('ref_axis',(-1.,0.,0.));
#20607=DIRECTION('',(0.,0.,-1.));
#20608=DIRECTION('center_axis',(0.,0.,-1.));
#20609=DIRECTION('ref_axis',(-1.,0.,0.));
#20610=DIRECTION('',(0.,0.,1.));
#20611=DIRECTION('center_axis',(0.,0.,-1.));
#20612=DIRECTION('ref_axis',(-1.,0.,0.));
#20613=DIRECTION('center_axis',(0.,0.,1.));
#20614=DIRECTION('ref_axis',(-1.,0.,0.));
#20615=DIRECTION('center_axis',(0.,0.,1.));
#20616=DIRECTION('ref_axis',(-1.,0.,0.));
#20617=DIRECTION('center_axis',(0.,0.,-1.));
#20618=DIRECTION('ref_axis',(-1.,0.,0.));
#20619=DIRECTION('center_axis',(0.,0.,-1.));
#20620=DIRECTION('ref_axis',(-1.,0.,0.));
#20621=DIRECTION('center_axis',(0.,0.,-1.));
#20622=DIRECTION('ref_axis',(-1.,0.,0.));
#20623=DIRECTION('center_axis',(0.,0.,-1.));
#20624=DIRECTION('ref_axis',(-1.,0.,0.));
#20625=DIRECTION('center_axis',(0.,0.,1.));
#20626=DIRECTION('ref_axis',(-1.,0.,0.));
#20627=DIRECTION('center_axis',(-1.,0.,0.));
#20628=DIRECTION('ref_axis',(0.,0.,1.));
#20629=DIRECTION('center_axis',(0.,0.,-1.));
#20630=DIRECTION('ref_axis',(1.,1.22464679914735E-16,0.));
#20631=DIRECTION('',(0.,0.,-1.));
#20632=DIRECTION('center_axis',(0.,0.,-1.));
#20633=DIRECTION('ref_axis',(-1.,0.,0.));
#20634=DIRECTION('',(0.,0.,-1.));
#20635=DIRECTION('center_axis',(0.,0.,-1.));
#20636=DIRECTION('ref_axis',(1.,1.22464679914735E-16,0.));
#20637=DIRECTION('center_axis',(0.,0.,1.));
#20638=DIRECTION('ref_axis',(-1.,0.,0.));
#20639=DIRECTION('center_axis',(0.,0.,-1.));
#20640=DIRECTION('ref_axis',(-1.,0.,0.));
#20641=DIRECTION('center_axis',(0.,0.,1.));
#20642=DIRECTION('ref_axis',(-1.,0.,0.));
#20643=DIRECTION('center_axis',(0.,0.,-1.));
#20644=DIRECTION('ref_axis',(-1.,0.,0.));
#20645=DIRECTION('center_axis',(0.,0.,-1.));
#20646=DIRECTION('ref_axis',(-1.,0.,0.));
#20647=DIRECTION('center_axis',(0.,0.,-1.));
#20648=DIRECTION('ref_axis',(-1.,0.,0.));
#20649=DIRECTION('center_axis',(0.,0.,-1.));
#20650=DIRECTION('ref_axis',(-1.,0.,0.));
#20651=DIRECTION('center_axis',(0.,0.,-1.));
#20652=DIRECTION('ref_axis',(-1.,0.,0.));
#20653=DIRECTION('center_axis',(0.,0.,-1.));
#20654=DIRECTION('ref_axis',(0.999962538604135,0.00865571420359059,0.));
#20655=DIRECTION('center_axis',(0.,0.,-1.));
#20656=DIRECTION('ref_axis',(-1.,0.,0.));
#20657=DIRECTION('center_axis',(0.,0.,-1.));
#20658=DIRECTION('ref_axis',(-1.,0.,0.));
#20659=DIRECTION('',(1.,0.,0.));
#20660=DIRECTION('',(1.,0.,0.));
#20661=DIRECTION('center_axis',(0.,0.,1.));
#20662=DIRECTION('ref_axis',(1.,0.,0.));
#20663=DIRECTION('center_axis',(0.,0.,1.));
#20664=DIRECTION('ref_axis',(1.,0.,0.));
#20665=DIRECTION('',(0.,0.,-1.));
#20666=DIRECTION('center_axis',(0.,0.,-1.));
#20667=DIRECTION('ref_axis',(1.,-5.55111512312578E-15,0.));
#20668=DIRECTION('',(0.,0.,1.));
#20669=DIRECTION('center_axis',(0.,0.,1.));
#20670=DIRECTION('ref_axis',(1.,0.,0.));
#20671=DIRECTION('center_axis',(0.,0.,1.));
#20672=DIRECTION('ref_axis',(1.,0.,0.));
#20673=DIRECTION('',(0.,0.,-1.));
#20674=DIRECTION('center_axis',(0.,0.,-1.));
#20675=DIRECTION('ref_axis',(1.,-4.16333634234433E-15,0.));
#20676=DIRECTION('',(0.,0.,1.));
#20677=DIRECTION('',(-1.,0.,0.));
#20678=DIRECTION('',(-1.,0.,0.));
#20679=DIRECTION('center_axis',(0.,0.,1.));
#20680=DIRECTION('ref_axis',(1.,0.,0.));
#20681=DIRECTION('center_axis',(0.,0.,1.));
#20682=DIRECTION('ref_axis',(-1.,0.,0.));
#20683=DIRECTION('',(0.,0.,1.));
#20684=DIRECTION('center_axis',(0.,0.,1.));
#20685=DIRECTION('ref_axis',(-1.,0.,0.));
#20686=DIRECTION('',(0.,0.,1.));
#20687=DIRECTION('center_axis',(0.,0.,1.));
#20688=DIRECTION('ref_axis',(-0.0126564647418527,-0.999919903742414,0.));
#20689=DIRECTION('center_axis',(0.,0.,-1.));
#20690=DIRECTION('ref_axis',(1.,0.,0.));
#20691=DIRECTION('',(0.,0.,1.));
#20692=DIRECTION('center_axis',(0.,0.,1.));
#20693=DIRECTION('ref_axis',(1.,0.,0.));
#20694=DIRECTION('',(0.,0.,-1.));
#20695=DIRECTION('center_axis',(0.,0.,1.));
#20696=DIRECTION('ref_axis',(1.,0.,0.));
#20697=DIRECTION('center_axis',(0.,0.,1.));
#20698=DIRECTION('ref_axis',(1.,0.,0.));
#20699=DIRECTION('',(0.,0.,1.));
#20700=DIRECTION('center_axis',(0.,0.,1.));
#20701=DIRECTION('ref_axis',(1.,0.,0.));
#20702=DIRECTION('',(0.,0.,1.));
#20703=DIRECTION('center_axis',(0.,0.,-1.));
#20704=DIRECTION('ref_axis',(-1.,0.,0.));
#20705=DIRECTION('center_axis',(0.,0.,1.));
#20706=DIRECTION('ref_axis',(1.,0.,0.));
#20707=DIRECTION('',(0.,0.,1.));
#20708=DIRECTION('',(0.,0.,1.));
#20709=DIRECTION('center_axis',(0.,0.,1.));
#20710=DIRECTION('ref_axis',(1.,0.,0.));
#20711=DIRECTION('center_axis',(0.,0.,-1.));
#20712=DIRECTION('ref_axis',(-1.,0.,0.));
#20713=DIRECTION('center_axis',(0.,0.,1.));
#20714=DIRECTION('ref_axis',(1.,0.,0.));
#20715=DIRECTION('',(0.,0.,-1.));
#20716=DIRECTION('',(0.,0.,-1.));
#20717=DIRECTION('center_axis',(0.,0.,1.));
#20718=DIRECTION('ref_axis',(1.,0.,0.));
#20719=DIRECTION('center_axis',(0.,0.,1.));
#20720=DIRECTION('ref_axis',(1.,0.,0.));
#20721=DIRECTION('center_axis',(0.,0.,1.));
#20722=DIRECTION('ref_axis',(1.,0.,0.));
#20723=DIRECTION('',(0.,0.,1.));
#20724=DIRECTION('',(0.,0.,-1.));
#20725=DIRECTION('center_axis',(0.,0.,1.));
#20726=DIRECTION('ref_axis',(1.,0.,0.));
#20727=DIRECTION('center_axis',(0.,0.,1.));
#20728=DIRECTION('ref_axis',(1.,0.,0.));
#20729=DIRECTION('center_axis',(0.,0.,1.));
#20730=DIRECTION('ref_axis',(1.,0.,0.));
#20731=DIRECTION('',(0.,0.,1.));
#20732=DIRECTION('center_axis',(0.,0.,1.));
#20733=DIRECTION('ref_axis',(1.,0.,0.));
#20734=DIRECTION('center_axis',(0.,0.,1.));
#20735=DIRECTION('ref_axis',(1.,0.,0.));
#20736=DIRECTION('',(0.,0.,1.));
#20737=DIRECTION('center_axis',(0.,0.,1.));
#20738=DIRECTION('ref_axis',(1.,0.,0.));
#20739=DIRECTION('center_axis',(0.,0.,1.));
#20740=DIRECTION('ref_axis',(1.,0.,0.));
#20741=DIRECTION('center_axis',(0.,0.,-1.));
#20742=DIRECTION('ref_axis',(1.,2.77555756156289E-15,0.));
#20743=DIRECTION('center_axis',(0.,0.,-1.));
#20744=DIRECTION('ref_axis',(1.,1.81922337360341E-15,0.));
#20745=DIRECTION('center_axis',(0.,0.,1.));
#20746=DIRECTION('ref_axis',(1.,0.,0.));
#20747=DIRECTION('center_axis',(0.,0.,1.));
#20748=DIRECTION('ref_axis',(1.,0.,0.));
#20749=DIRECTION('center_axis',(0.,0.,1.));
#20750=DIRECTION('ref_axis',(1.,0.,0.));
#20751=DIRECTION('center_axis',(0.,0.,-1.));
#20752=DIRECTION('ref_axis',(1.,0.,0.));
#20753=DIRECTION('center_axis',(0.,0.,1.));
#20754=DIRECTION('ref_axis',(1.,0.,0.));
#20755=DIRECTION('center_axis',(0.,0.,1.));
#20756=DIRECTION('ref_axis',(1.,0.,0.));
#20757=DIRECTION('center_axis',(0.,0.,-1.));
#20758=DIRECTION('ref_axis',(1.,-1.38777878078144E-15,0.));
#20759=DIRECTION('',(-0.766044443118986,0.64278760968653,0.));
#20760=DIRECTION('',(0.64278760968653,0.766044443118986,0.));
#20761=DIRECTION('center_axis',(0.,0.,1.));
#20762=DIRECTION('ref_axis',(1.,0.,0.));
#20763=DIRECTION('',(0.984807753012206,0.17364817766694,0.));
#20764=DIRECTION('',(-0.17364817766694,0.984807753012206,0.));
#20765=DIRECTION('',(0.984807753012206,0.17364817766694,0.));
#20766=DIRECTION('',(0.866025403784443,-0.499999999999992,0.));
#20767=DIRECTION('',(0.499999999999992,0.866025403784443,0.));
#20768=DIRECTION('',(0.866025403784443,-0.499999999999992,0.));
#20769=DIRECTION('center_axis',(0.,0.,1.));
#20770=DIRECTION('ref_axis',(1.,0.,0.));
#20771=DIRECTION('',(0.342020143325676,-0.939692620785906,0.));
#20772=DIRECTION('',(0.939692620785906,0.342020143325676,0.));
#20773=DIRECTION('',(0.342020143325676,-0.939692620785906,0.));
#20774=DIRECTION('center_axis',(0.,0.,1.));
#20775=DIRECTION('ref_axis',(1.,0.,0.));
#20776=DIRECTION('',(-0.342020143325663,-0.93969262078591,0.));
#20777=DIRECTION('',(0.93969262078591,-0.342020143325663,0.));
#20778=DIRECTION('',(-0.342020143325663,-0.93969262078591,0.));
#20779=DIRECTION('center_axis',(0.,0.,1.));
#20780=DIRECTION('ref_axis',(1.,0.,0.));
#20781=DIRECTION('',(-0.866025403784436,-0.500000000000004,0.));
#20782=DIRECTION('',(0.500000000000004,-0.866025403784436,0.));
#20783=DIRECTION('',(-0.866025403784436,-0.500000000000004,0.));
#20784=DIRECTION('',(0.500000000000004,-0.866025403784436,0.));
#20785=DIRECTION('center_axis',(0.,0.,1.));
#20786=DIRECTION('ref_axis',(1.,0.,0.));
#20787=DIRECTION('',(-0.173648177666927,-0.984807753012209,0.));
#20788=DIRECTION('',(-0.984807753012209,0.173648177666927,0.));
#20789=DIRECTION('',(-0.173648177666927,-0.984807753012209,0.));
#20790=DIRECTION('',(-0.984807753012209,0.173648177666927,0.));
#20791=DIRECTION('',(-0.173648177666927,-0.984807753012209,0.));
#20792=DIRECTION('center_axis',(0.,0.,1.));
#20793=DIRECTION('ref_axis',(1.,0.,0.));
#20794=DIRECTION('',(-0.64278760968654,0.766044443118977,0.));
#20795=DIRECTION('',(-0.766044443118977,-0.64278760968654,0.));
#20796=DIRECTION('',(-0.64278760968654,0.766044443118977,0.));
#20797=DIRECTION('center_axis',(0.,0.,1.));
#20798=DIRECTION('ref_axis',(1.,0.,0.));
#20799=DIRECTION('',(0.,1.,0.));
#20800=DIRECTION('',(-1.,0.,0.));
#20801=DIRECTION('',(0.,1.,0.));
#20802=DIRECTION('center_axis',(0.,0.,1.));
#20803=DIRECTION('ref_axis',(1.,0.,0.));
#20804=DIRECTION('',(0.64278760968653,0.766044443118986,0.));
#20805=DIRECTION('center_axis',(0.,0.,1.));
#20806=DIRECTION('ref_axis',(1.,0.,0.));
#20807=DIRECTION('',(0.,0.,1.));
#20808=DIRECTION('center_axis',(0.,0.,1.));
#20809=DIRECTION('ref_axis',(1.,0.,0.));
#20810=DIRECTION('',(0.,0.,1.));
#20811=DIRECTION('center_axis',(0.,0.,1.));
#20812=DIRECTION('ref_axis',(1.,0.,0.));
#20813=DIRECTION('',(0.,0.,1.));
#20814=DIRECTION('center_axis',(0.,0.,1.));
#20815=DIRECTION('ref_axis',(1.,0.,0.));
#20816=DIRECTION('',(0.,0.,1.));
#20817=DIRECTION('center_axis',(0.,0.,1.));
#20818=DIRECTION('ref_axis',(1.,0.,0.));
#20819=DIRECTION('',(0.,0.,1.));
#20820=DIRECTION('center_axis',(0.,0.,1.));
#20821=DIRECTION('ref_axis',(1.,0.,0.));
#20822=DIRECTION('',(0.,0.,1.));
#20823=DIRECTION('center_axis',(0.,0.,1.));
#20824=DIRECTION('ref_axis',(1.,0.,0.));
#20825=DIRECTION('',(0.,0.,1.));
#20826=DIRECTION('center_axis',(0.,0.,1.));
#20827=DIRECTION('ref_axis',(1.,0.,0.));
#20828=DIRECTION('',(0.,0.,1.));
#20829=DIRECTION('center_axis',(0.,0.,1.));
#20830=DIRECTION('ref_axis',(-0.988219026491317,-0.153046253402539,0.));
#20831=DIRECTION('',(0.,0.,1.));
#20832=DIRECTION('center_axis',(0.,0.,1.));
#20833=DIRECTION('ref_axis',(1.,0.,0.));
#20834=DIRECTION('',(0.,0.,-1.));
#20835=DIRECTION('center_axis',(0.,0.,1.));
#20836=DIRECTION('ref_axis',(1.,0.,0.));
#20837=DIRECTION('',(0.,0.,1.));
#20838=DIRECTION('',(0.,0.,1.));
#20839=DIRECTION('center_axis',(0.,0.,1.));
#20840=DIRECTION('ref_axis',(1.,0.,0.));
#20841=DIRECTION('center_axis',(0.,0.,1.));
#20842=DIRECTION('ref_axis',(1.,0.,0.));
#20843=DIRECTION('',(0.,0.,1.));
#20844=DIRECTION('center_axis',(0.,0.,1.));
#20845=DIRECTION('ref_axis',(1.,0.,0.));
#20846=DIRECTION('',(0.,0.,1.));
#20847=DIRECTION('center_axis',(0.,0.,1.));
#20848=DIRECTION('ref_axis',(1.,0.,0.));
#20849=DIRECTION('',(0.,0.,1.));
#20850=DIRECTION('center_axis',(0.,0.,1.));
#20851=DIRECTION('ref_axis',(1.,0.,0.));
#20852=DIRECTION('',(0.,0.,1.));
#20853=DIRECTION('center_axis',(0.,0.,1.));
#20854=DIRECTION('ref_axis',(1.,0.,0.));
#20855=DIRECTION('center_axis',(0.,0.,1.));
#20856=DIRECTION('ref_axis',(1.,0.,0.));
#20857=DIRECTION('center_axis',(0.,0.,-1.));
#20858=DIRECTION('ref_axis',(-1.,0.,0.));
#20859=DIRECTION('',(0.,0.,-1.));
#20860=DIRECTION('center_axis',(0.,0.,-1.));
#20861=DIRECTION('ref_axis',(1.,1.81922337360341E-15,0.));
#20862=DIRECTION('',(0.,0.,-1.));
#20863=DIRECTION('center_axis',(0.,0.,-1.));
#20864=DIRECTION('ref_axis',(-1.,0.,0.));
#20865=DIRECTION('center_axis',(0.,0.,1.));
#20866=DIRECTION('ref_axis',(1.,0.,0.));
#20867=DIRECTION('',(0.,0.,-1.));
#20868=DIRECTION('center_axis',(0.,0.,-1.));
#20869=DIRECTION('ref_axis',(-1.,0.,0.));
#20870=DIRECTION('center_axis',(0.,0.,1.));
#20871=DIRECTION('ref_axis',(1.,0.,0.));
#20872=DIRECTION('center_axis',(0.,0.,-1.));
#20873=DIRECTION('ref_axis',(-1.,0.,0.));
#20874=DIRECTION('center_axis',(0.,0.,-1.));
#20875=DIRECTION('ref_axis',(1.,0.,0.));
#20876=DIRECTION('',(0.,0.,-1.));
#20877=DIRECTION('center_axis',(0.,0.,-1.));
#20878=DIRECTION('ref_axis',(-1.,0.,0.));
#20879=DIRECTION('center_axis',(0.,0.,1.));
#20880=DIRECTION('ref_axis',(1.,0.,0.));
#20881=DIRECTION('',(0.,0.,-1.));
#20882=DIRECTION('center_axis',(0.,0.,-1.));
#20883=DIRECTION('ref_axis',(-1.,0.,0.));
#20884=DIRECTION('center_axis',(0.,0.,1.));
#20885=DIRECTION('ref_axis',(1.,0.,0.));
#20886=DIRECTION('',(0.,0.,1.));
#20887=DIRECTION('center_axis',(0.,0.,1.));
#20888=DIRECTION('ref_axis',(1.,0.,0.));
#20889=DIRECTION('center_axis',(0.,0.,1.));
#20890=DIRECTION('ref_axis',(1.,0.,0.));
#20891=DIRECTION('center_axis',(0.,0.,1.));
#20892=DIRECTION('ref_axis',(1.,0.,0.));
#20893=DIRECTION('center_axis',(0.,0.,1.));
#20894=DIRECTION('ref_axis',(1.,0.,0.));
#20895=DIRECTION('',(0.,1.,0.));
#20896=DIRECTION('',(-1.,0.,0.));
#20897=DIRECTION('',(0.,-1.,0.));
#20898=DIRECTION('center_axis',(0.,0.,1.));
#20899=DIRECTION('ref_axis',(1.,0.,0.));
#20900=DIRECTION('',(-0.64278760968653,-0.766044443118986,0.));
#20901=DIRECTION('',(-0.766044443118986,0.64278760968653,0.));
#20902=DIRECTION('',(-0.64278760968653,-0.766044443118986,0.));
#20903=DIRECTION('',(0.,-1.,0.));
#20904=DIRECTION('',(-1.,0.,0.));
#20905=DIRECTION('',(0.,-1.,0.));
#20906=DIRECTION('',(0.64278760968654,-0.766044443118977,0.));
#20907=DIRECTION('',(-0.766044443118977,-0.64278760968654,0.));
#20908=DIRECTION('',(0.64278760968654,-0.766044443118977,0.));
#20909=DIRECTION('',(-0.173648177666927,-0.984807753012209,0.));
#20910=DIRECTION('',(0.984807753012209,-0.173648177666927,0.));
#20911=DIRECTION('',(-0.173648177666927,-0.984807753012209,0.));
#20912=DIRECTION('',(0.984807753012209,-0.173648177666927,0.));
#20913=DIRECTION('',(-0.173648177666927,-0.984807753012209,0.));
#20914=DIRECTION('',(0.500000000000004,-0.866025403784436,0.));
#20915=DIRECTION('',(0.866025403784436,0.500000000000004,0.));
#20916=DIRECTION('',(0.500000000000004,-0.866025403784436,0.));
#20917=DIRECTION('',(0.866025403784436,0.500000000000004,0.));
#20918=DIRECTION('',(0.342020143325663,0.93969262078591,0.));
#20919=DIRECTION('',(0.93969262078591,-0.342020143325663,0.));
#20920=DIRECTION('',(0.342020143325663,0.93969262078591,0.));
#20921=DIRECTION('',(-0.342020143325676,0.939692620785906,0.));
#20922=DIRECTION('',(0.939692620785906,0.342020143325676,0.));
#20923=DIRECTION('',(-0.342020143325676,0.939692620785906,0.));
#20924=DIRECTION('',(-0.866025403784443,0.499999999999992,0.));
#20925=DIRECTION('',(0.499999999999992,0.866025403784443,0.));
#20926=DIRECTION('',(-0.866025403784443,0.499999999999992,0.));
#20927=DIRECTION('',(-0.984807753012206,-0.17364817766694,0.));
#20928=DIRECTION('',(-0.17364817766694,0.984807753012206,0.));
#20929=DIRECTION('',(-0.984807753012206,-0.17364817766694,0.));
#20930=DIRECTION('',(0.,1.,0.));
#20931=DIRECTION('',(0.,-1.,0.));
#20932=DIRECTION('',(-1.,0.,0.));
#20933=DIRECTION('center_axis',(0.,0.,1.));
#20934=DIRECTION('ref_axis',(-1.,1.45473230946492E-15,0.));
#20935=DIRECTION('center_axis',(0.,-0.152153200171805,-0.98835692119673));
#20936=DIRECTION('ref_axis',(0.,0.98835692119673,-0.152153200171805));
#20937=DIRECTION('',(0.,-0.98835692119673,0.152153200171805));
#20938=DIRECTION('',(0.,-0.98835692119673,0.152153200171805));
#20939=DIRECTION('center_axis',(-1.,0.,0.));
#20940=DIRECTION('ref_axis',(0.,0.,1.));
#20941=DIRECTION('center_axis',(-1.,0.,0.));
#20942=DIRECTION('ref_axis',(0.,0.,1.));
#20943=DIRECTION('center_axis',(0.0978021918445919,-0.11655611349438,-0.98835692119673));
#20944=DIRECTION('ref_axis',(1.08893713285454E-18,0.993118054469193,-0.117117589999644));
#20945=DIRECTION('',(0.635303582893194,-0.757125327300936,0.152153200171805));
#20946=DIRECTION('',(0.635303582893194,-0.757125327300936,0.152153200171805));
#20947=DIRECTION('center_axis',(-0.766044443118977,-0.64278760968654,0.));
#20948=DIRECTION('ref_axis',(0.,0.,1.));
#20949=DIRECTION('center_axis',(-0.766044443118977,-0.64278760968654,0.));
#20950=DIRECTION('ref_axis',(0.,0.,1.));
#20951=DIRECTION('center_axis',(-0.984807753012209,0.173648177666927,0.));
#20952=DIRECTION('ref_axis',(-0.173648177666927,-0.984807753012209,0.));
#20953=DIRECTION('',(0.,0.,-1.));
#20954=DIRECTION('center_axis',(-0.984807753012209,0.173648177666927,0.));
#20955=DIRECTION('ref_axis',(-0.173648177666927,-0.984807753012209,0.));
#20956=DIRECTION('',(0.,0.,-1.));
#20957=DIRECTION('center_axis',(0.149841651174812,-0.0264211259360251,-0.98835692119673));
#20958=DIRECTION('ref_axis',(-0.988702075986957,-2.27568915914982E-19,-0.149893978995429));
#20959=DIRECTION('',(0.973341558737816,-0.171626378250307,0.152153200171805));
#20960=DIRECTION('',(0.973341558737816,-0.171626378250307,0.152153200171805));
#20961=DIRECTION('center_axis',(-0.173648177666927,-0.984807753012209,0.));
#20962=DIRECTION('ref_axis',(0.,0.,1.));
#20963=DIRECTION('center_axis',(-0.173648177666927,-0.984807753012209,0.));
#20964=DIRECTION('ref_axis',(0.,0.,1.));
#20965=DIRECTION('center_axis',(-0.866025403784436,-0.500000000000004,0.));
#20966=DIRECTION('ref_axis',(0.500000000000004,-0.866025403784436,0.));
#20967=DIRECTION('',(0.,0.,-1.));
#20968=DIRECTION('center_axis',(0.131768536615881,0.0760766000859029,-0.98835692119673));
#20969=DIRECTION('ref_axis',(-0.991229527971275,-4.70862379419472E-20,-0.132151514852626));
#20970=DIRECTION('',(0.85594220176254,0.494178460598369,0.152153200171805));
#20971=DIRECTION('',(0.85594220176254,0.494178460598369,0.152153200171805));
#20972=DIRECTION('center_axis',(0.500000000000004,-0.866025403784436,0.));
#20973=DIRECTION('ref_axis',(0.,0.,1.));
#20974=DIRECTION('center_axis',(0.500000000000004,-0.866025403784436,0.));
#20975=DIRECTION('ref_axis',(0.,0.,1.));
#20976=DIRECTION('center_axis',(0.0520394593302189,0.142977239430406,-0.98835692119673));
#20977=DIRECTION('ref_axis',(5.2259940538791E-19,0.98969793283463,0.143171232246077));
#20978=DIRECTION('',(0.338037975844617,0.928751705551249,0.152153200171805));
#20979=DIRECTION('',(0.338037975844617,0.928751705551249,0.152153200171805));
#20980=DIRECTION('center_axis',(0.939692620785911,-0.342020143325663,0.));
#20981=DIRECTION('ref_axis',(0.,0.,1.));
#20982=DIRECTION('center_axis',(0.939692620785911,-0.342020143325663,0.));
#20983=DIRECTION('ref_axis',(0.,0.,1.));
#20984=DIRECTION('center_axis',(-0.0520394593302208,0.142977239430406,-0.98835692119673));
#20985=DIRECTION('ref_axis',(-3.0713028184418E-19,0.98969793283463,0.143171232246077));
#20986=DIRECTION('',(-0.338037975844629,0.928751705551244,0.152153200171805));
#20987=DIRECTION('',(-0.338037975844629,0.928751705551244,0.152153200171805));
#20988=DIRECTION('center_axis',(0.939692620785906,0.342020143325676,0.));
#20989=DIRECTION('ref_axis',(0.,0.,1.));
#20990=DIRECTION('center_axis',(0.939692620785906,0.342020143325676,0.));
#20991=DIRECTION('ref_axis',(0.,0.,1.));
#20992=DIRECTION('center_axis',(-0.131768536615882,0.076076600085901,-0.98835692119673));
#20993=DIRECTION('ref_axis',(-0.991229527971275,2.06899881612888E-19,0.132151514852627));
#20994=DIRECTION('',(-0.855942201762547,0.494178460598357,0.152153200171805));
#20995=DIRECTION('',(-0.855942201762547,0.494178460598357,0.152153200171805));
#20996=DIRECTION('center_axis',(0.499999999999992,0.866025403784443,0.));
#20997=DIRECTION('ref_axis',(0.,0.,1.));
#20998=DIRECTION('center_axis',(0.499999999999992,0.866025403784443,0.));
#20999=DIRECTION('ref_axis',(0.,0.,1.));
#21000=DIRECTION('center_axis',(-0.149841651174811,-0.0264211259360271,
-0.98835692119673));
#21001=DIRECTION('ref_axis',(-0.988702075986957,-4.57290035202453E-19,0.149893978995429));
#21002=DIRECTION('',(-0.973341558737814,-0.17162637825032,0.152153200171805));
#21003=DIRECTION('',(-0.973341558737814,-0.17162637825032,0.152153200171805));
#21004=DIRECTION('center_axis',(-0.17364817766694,0.984807753012206,0.));
#21005=DIRECTION('ref_axis',(0.,0.,1.));
#21006=DIRECTION('center_axis',(-0.17364817766694,0.984807753012206,0.));
#21007=DIRECTION('ref_axis',(0.,0.,1.));
#21008=DIRECTION('center_axis',(-0.0978021918445904,-0.116556113494382,
-0.98835692119673));
#21009=DIRECTION('ref_axis',(-4.42616424608758E-19,0.993118054469193,-0.117117589999646));
#21010=DIRECTION('',(-0.635303582893184,-0.757125327300944,0.152153200171805));
#21011=DIRECTION('',(-0.635303582893184,-0.757125327300944,0.152153200171805));
#21012=DIRECTION('center_axis',(-0.766044443118986,0.64278760968653,0.));
#21013=DIRECTION('ref_axis',(0.,0.,1.));
#21014=DIRECTION('center_axis',(-0.766044443118986,0.64278760968653,0.));
#21015=DIRECTION('ref_axis',(0.,0.,1.));
#21016=DIRECTION('center_axis',(0.,0.,1.));
#21017=DIRECTION('ref_axis',(-0.957942704987207,0.286959533665974,0.));
#21018=DIRECTION('center_axis',(0.,0.,1.));
#21019=DIRECTION('ref_axis',(-0.957942704987206,-0.286959533665975,0.));
#21020=DIRECTION('center_axis',(1.,0.,0.));
#21021=DIRECTION('ref_axis',(0.,0.,-1.));
#21022=DIRECTION('',(0.,0.,1.));
#21023=DIRECTION('center_axis',(-1.,0.,0.));
#21024=DIRECTION('ref_axis',(0.,0.,1.));
#21025=DIRECTION('',(0.,0.,1.));
#21026=DIRECTION('center_axis',(0.,1.,0.));
#21027=DIRECTION('ref_axis',(0.,0.,1.));
#21028=DIRECTION('axis',(0.,0.,1.));
#21029=DIRECTION('refdir',(1.,0.,0.));
#21030=DIRECTION('center_axis',(0.,0.,1.));
#21031=DIRECTION('ref_axis',(-1.,1.22464679914735E-16,0.));
#21032=DIRECTION('center_axis',(-1.,6.12323399573677E-17,0.));
#21033=DIRECTION('ref_axis',(6.12323399573677E-17,1.,0.));
#21034=DIRECTION('center_axis',(0.,0.,1.));
#21035=DIRECTION('ref_axis',(-1.,1.22464679914735E-16,0.));
#21036=DIRECTION('center_axis',(0.,0.,1.));
#21037=DIRECTION('ref_axis',(-1.,1.22464679914735E-16,0.));
#21038=DIRECTION('center_axis',(1.,0.,0.));
#21039=DIRECTION('ref_axis',(0.,0.,-1.));
#21040=DIRECTION('center_axis',(1.,0.,0.));
#21041=DIRECTION('ref_axis',(0.,0.,-1.));
#21042=DIRECTION('center_axis',(-1.,6.12323399573677E-17,0.));
#21043=DIRECTION('ref_axis',(6.12323399573677E-17,1.,0.));
#21044=DIRECTION('center_axis',(0.,0.,1.));
#21045=DIRECTION('ref_axis',(-1.,1.22464679914735E-16,0.));
#21046=DIRECTION('center_axis',(1.,2.55123084520842E-16,0.));
#21047=DIRECTION('ref_axis',(-2.55123084520842E-16,1.,0.));
#21048=DIRECTION('center_axis',(1.,2.55123084520842E-16,0.));
#21049=DIRECTION('ref_axis',(-2.55123084520842E-16,1.,0.));
#21050=DIRECTION('center_axis',(0.,0.,-1.));
#21051=DIRECTION('ref_axis',(-1.,1.22464679914735E-16,0.));
#21052=DIRECTION('center_axis',(0.,0.,-1.));
#21053=DIRECTION('ref_axis',(-1.,1.22464679914735E-16,0.));
#21054=DIRECTION('center_axis',(-1.,-4.38820104392945E-16,0.));
#21055=DIRECTION('ref_axis',(4.38820104392945E-16,-1.,0.));
#21056=DIRECTION('center_axis',(-1.,-4.38820104392945E-16,0.));
#21057=DIRECTION('ref_axis',(4.38820104392945E-16,-1.,0.));
#21058=DIRECTION('center_axis',(-0.582556010419622,-0.750905958805901,0.311076736117899));
#21059=DIRECTION('ref_axis',(0.790107291694676,-0.612968569839355,-3.50006659356662E-16));
#21060=DIRECTION('center_axis',(-0.582614729034438,0.755300040476885,-0.300136512886627));
#21061=DIRECTION('ref_axis',(-0.791805223116158,-0.610773680380852,1.37374746571133E-16));
#21062=DIRECTION('center_axis',(1.,0.,0.));
#21063=DIRECTION('ref_axis',(0.,0.,-1.));
#21064=DIRECTION('',(1.,0.,0.));
#21065=DIRECTION('center_axis',(1.,4.38820104392945E-16,0.));
#21066=DIRECTION('ref_axis',(-4.38820104392945E-16,1.,0.));
#21067=DIRECTION('center_axis',(-1.,0.,0.));
#21068=DIRECTION('ref_axis',(0.,0.,1.));
#21069=DIRECTION('center_axis',(-1.,-4.38820104392945E-16,0.));
#21070=DIRECTION('ref_axis',(4.38820104392945E-16,-1.,0.));
#21071=DIRECTION('',(-1.,0.,0.));
#21072=DIRECTION('center_axis',(-0.582556010419622,-0.750905958805901,0.311076736117899));
#21073=DIRECTION('ref_axis',(0.790107291694676,-0.612968569839355,-4.40287716331881E-16));
#21074=DIRECTION('center_axis',(-0.582614729034438,0.755300040476885,-0.300136512886627));
#21075=DIRECTION('ref_axis',(-0.791805223116158,-0.610773680380852,2.90913046502425E-16));
#21076=DIRECTION('center_axis',(1.,0.,0.));
#21077=DIRECTION('ref_axis',(0.,0.,-1.));
#21078=DIRECTION('center_axis',(1.,4.38820104392945E-16,0.));
#21079=DIRECTION('ref_axis',(-4.38820104392945E-16,1.,0.));
#21080=DIRECTION('',(-1.,0.,0.));
#21081=DIRECTION('center_axis',(-1.,0.,0.));
#21082=DIRECTION('ref_axis',(0.,0.,1.));
#21083=DIRECTION('',(1.,0.,0.));
#21084=DIRECTION('center_axis',(-1.,-4.38820104392945E-16,0.));
#21085=DIRECTION('ref_axis',(4.38820104392945E-16,-1.,0.));
#21086=DIRECTION('center_axis',(1.,4.38820104392945E-16,0.));
#21087=DIRECTION('ref_axis',(-4.38820104392945E-16,1.,0.));
#21088=DIRECTION('center_axis',(-1.,-4.38820104392945E-16,0.));
#21089=DIRECTION('ref_axis',(4.38820104392945E-16,-1.,0.));
#21090=DIRECTION('center_axis',(0.,0.,1.));
#21091=DIRECTION('ref_axis',(-0.999999999995711,2.92869692484868E-6,0.));
#21092=DIRECTION('center_axis',(0.,0.,1.));
#21093=DIRECTION('ref_axis',(-0.999999999989654,4.54879961062145E-6,0.));
#21094=DIRECTION('axis',(0.,0.,1.));
#21095=DIRECTION('refdir',(1.,0.,0.));
#21096=DIRECTION('center_axis',(0.,1.,0.));
#21097=DIRECTION('ref_axis',(0.,0.,1.));
#21098=DIRECTION('center_axis',(0.,1.,0.));
#21099=DIRECTION('ref_axis',(0.,0.,-1.));
#21100=DIRECTION('',(0.,1.,0.));
#21101=DIRECTION('center_axis',(0.,1.,0.));
#21102=DIRECTION('ref_axis',(0.,0.,-1.));
#21103=DIRECTION('center_axis',(0.,1.,0.));
#21104=DIRECTION('ref_axis',(0.,0.,1.));
#21105=DIRECTION('center_axis',(0.,1.,0.));
#21106=DIRECTION('ref_axis',(0.,0.,-1.));
#21107=DIRECTION('',(0.,1.,0.));
#21108=DIRECTION('center_axis',(0.,1.,0.));
#21109=DIRECTION('ref_axis',(0.,0.,-1.));
#21110=DIRECTION('center_axis',(0.,1.,0.));
#21111=DIRECTION('ref_axis',(0.,0.,1.));
#21112=DIRECTION('center_axis',(0.,1.,0.));
#21113=DIRECTION('ref_axis',(0.,0.,1.));
#21114=DIRECTION('',(0.,1.,0.));
#21115=DIRECTION('center_axis',(0.,1.,0.));
#21116=DIRECTION('ref_axis',(0.,0.,1.));
#21117=DIRECTION('center_axis',(0.,1.,0.));
#21118=DIRECTION('ref_axis',(0.,0.,1.));
#21119=DIRECTION('center_axis',(0.,1.,0.));
#21120=DIRECTION('ref_axis',(0.,0.,1.));
#21121=DIRECTION('',(0.,1.,0.));
#21122=DIRECTION('center_axis',(0.,1.,0.));
#21123=DIRECTION('ref_axis',(0.,0.,1.));
#21124=DIRECTION('center_axis',(-1.,0.,-1.12538885307499E-16));
#21125=DIRECTION('ref_axis',(-1.12538885307499E-16,0.,1.));
#21126=DIRECTION('',(0.,-1.,0.));
#21127=DIRECTION('',(-1.14004428052113E-16,0.,1.));
#21128=DIRECTION('',(0.,-1.,0.));
#21129=DIRECTION('',(1.14004428052113E-16,0.,-1.));
#21130=DIRECTION('',(0.,-1.,0.));
#21131=DIRECTION('',(-1.32743918944454E-16,0.,1.));
#21132=DIRECTION('',(0.,1.,0.));
#21133=DIRECTION('',(1.38777878078144E-16,0.,-1.));
#21134=DIRECTION('',(0.,1.,0.));
#21135=DIRECTION('',(-9.28250249804007E-17,0.565386313251385,0.824826234299083));
#21136=DIRECTION('',(0.,1.,0.));
#21137=DIRECTION('',(1.25247756392721E-16,0.,-1.));
#21138=DIRECTION('center_axis',(1.,0.,-1.12538885307499E-16));
#21139=DIRECTION('ref_axis',(1.12538885307499E-16,0.,1.));
#21140=DIRECTION('',(0.,1.,0.));
#21141=DIRECTION('',(-1.12538885307499E-16,0.,-1.));
#21142=DIRECTION('',(0.,-1.,0.));
#21143=DIRECTION('',(-1.25247756392721E-16,0.,-1.));
#21144=DIRECTION('',(0.,1.,0.));
#21145=DIRECTION('',(9.28250249804007E-17,0.565386313251385,0.824826234299083));
#21146=DIRECTION('',(0.,1.,0.));
#21147=DIRECTION('',(1.38777878078144E-16,0.,1.));
#21148=DIRECTION('',(0.,1.,0.));
#21149=DIRECTION('',(1.32743918944454E-16,0.,1.));
#21150=DIRECTION('',(0.,-1.,0.));
#21151=DIRECTION('',(1.12538885307499E-16,0.,1.));
#21152=DIRECTION('center_axis',(0.,0.,1.));
#21153=DIRECTION('ref_axis',(1.,0.,0.));
#21154=DIRECTION('',(1.,0.,0.));
#21155=DIRECTION('',(0.,1.,0.));
#21156=DIRECTION('',(1.,0.,0.));
#21157=DIRECTION('center_axis',(-1.,0.,9.63735264431558E-17));
#21158=DIRECTION('ref_axis',(9.63735264431558E-17,0.,1.));
#21159=DIRECTION('',(9.63735264431558E-17,0.,1.));
#21160=DIRECTION('',(0.,1.,0.));
#21161=DIRECTION('',(9.63735264431558E-17,0.,1.));
#21162=DIRECTION('center_axis',(0.,0.,1.));
#21163=DIRECTION('ref_axis',(1.,0.,0.));
#21164=DIRECTION('',(1.,0.,0.));
#21165=DIRECTION('',(0.,1.,0.));
#21166=DIRECTION('',(1.,0.,0.));
#21167=DIRECTION('center_axis',(1.,0.,0.));
#21168=DIRECTION('ref_axis',(0.,0.,-1.));
#21169=DIRECTION('',(0.,0.,-1.));
#21170=DIRECTION('',(0.,1.,0.));
#21171=DIRECTION('',(0.,0.,-1.));
#21172=DIRECTION('center_axis',(0.,0.,1.));
#21173=DIRECTION('ref_axis',(1.,0.,0.));
#21174=DIRECTION('',(1.,0.,0.));
#21175=DIRECTION('',(1.,0.,0.));
#21176=DIRECTION('center_axis',(0.,0.,-1.));
#21177=DIRECTION('ref_axis',(-1.,0.,0.));
#21178=DIRECTION('',(-1.,0.,0.));
#21179=DIRECTION('',(0.,1.,0.));
#21180=DIRECTION('',(-1.,0.,0.));
#21181=DIRECTION('center_axis',(1.,0.,0.));
#21182=DIRECTION('ref_axis',(0.,0.,-1.));
#21183=DIRECTION('',(0.,0.,-1.));
#21184=DIRECTION('',(0.,1.,0.));
#21185=DIRECTION('',(0.,0.,-1.));
#21186=DIRECTION('center_axis',(0.,0.,-1.));
#21187=DIRECTION('ref_axis',(-1.,0.,0.));
#21188=DIRECTION('',(-1.,0.,0.));
#21189=DIRECTION('',(0.,1.,0.));
#21190=DIRECTION('',(-1.,0.,0.));
#21191=DIRECTION('center_axis',(-1.,0.,0.));
#21192=DIRECTION('ref_axis',(0.,0.,1.));
#21193=DIRECTION('',(0.,0.,1.));
#21194=DIRECTION('',(0.,1.,0.));
#21195=DIRECTION('',(0.,0.,1.));
#21196=DIRECTION('center_axis',(0.,0.,-1.));
#21197=DIRECTION('ref_axis',(-1.,0.,0.));
#21198=DIRECTION('',(-1.,0.,0.));
#21199=DIRECTION('',(-1.,0.,0.));
#21200=DIRECTION('center_axis',(0.,1.,0.));
#21201=DIRECTION('ref_axis',(0.,0.,1.));
#21202=DIRECTION('center_axis',(0.,1.,0.));
#21203=DIRECTION('ref_axis',(0.,0.,1.));
#21204=DIRECTION('',(-1.,0.,-1.38777878078144E-16));
#21205=DIRECTION('',(-1.32743918944454E-16,0.,1.));
#21206=DIRECTION('',(-1.,0.,-1.38777878078144E-16));
#21207=DIRECTION('',(1.,0.,-1.38777878078144E-16));
#21208=DIRECTION('',(1.32743918944454E-16,0.,1.));
#21209=DIRECTION('',(1.,0.,-1.38777878078144E-16));
#21210=DIRECTION('center_axis',(-7.84631128474524E-17,-0.824826234299083,
0.565386313251385));
#21211=DIRECTION('ref_axis',(-6.77673776348631E-34,-0.565386313251385,-0.824826234299084));
#21212=DIRECTION('',(-9.28250249804007E-17,0.565386313251385,0.824826234299083));
#21213=DIRECTION('',(-1.,0.,-1.38777878078144E-16));
#21214=DIRECTION('center_axis',(1.38777878078144E-16,0.,-1.));
#21215=DIRECTION('ref_axis',(-1.,0.,-1.38777878078145E-16));
#21216=DIRECTION('',(-1.,0.,-1.38777878078144E-16));
#21217=DIRECTION('',(0.,-1.,0.));
#21218=DIRECTION('center_axis',(0.,-1.,0.));
#21219=DIRECTION('ref_axis',(0.,0.,-1.));
#21220=DIRECTION('',(1.,0.,1.32222068111359E-16));
#21221=DIRECTION('',(1.,0.,-1.38777878078144E-16));
#21222=DIRECTION('',(1.41190366869118E-16,0.,1.));
#21223=DIRECTION('',(-1.,0.,-1.38777878078144E-16));
#21224=DIRECTION('',(-1.41190366869118E-16,0.,1.));
#21225=DIRECTION('center_axis',(1.38777878078144E-16,0.,-1.));
#21226=DIRECTION('ref_axis',(-1.,0.,-1.38777878078145E-16));
#21227=DIRECTION('',(0.,-1.,0.));
#21228=DIRECTION('',(1.,0.,-1.38777878078144E-16));
#21229=DIRECTION('',(1.,0.,1.32222068111359E-16));
#21230=DIRECTION('',(-1.,0.,-1.38777878078144E-16));
#21231=DIRECTION('',(0.,-1.,0.));
#21232=DIRECTION('center_axis',(0.,1.,0.));
#21233=DIRECTION('ref_axis',(0.,0.,1.));
#21234=DIRECTION('',(-1.,0.,-1.38777878078144E-16));
#21235=DIRECTION('',(1.25247756392721E-16,0.,-1.));
#21236=DIRECTION('center_axis',(-1.38777878078144E-16,0.,1.));
#21237=DIRECTION('ref_axis',(1.,0.,1.38777878078145E-16));
#21238=DIRECTION('',(0.,1.,0.));
#21239=DIRECTION('center_axis',(-1.,0.,-1.12538885307499E-16));
#21240=DIRECTION('ref_axis',(-1.12538885307499E-16,0.,1.));
#21241=DIRECTION('center_axis',(-7.84631128474524E-17,0.824826234299083,
-0.565386313251385));
#21242=DIRECTION('ref_axis',(-6.77673776348631E-34,0.565386313251385,0.824826234299084));
#21243=DIRECTION('',(1.,0.,-1.38777878078144E-16));
#21244=DIRECTION('',(9.28250249804007E-17,0.565386313251385,0.824826234299083));
#21245=DIRECTION('center_axis',(-1.38777878078144E-16,0.,-1.));
#21246=DIRECTION('ref_axis',(-1.,0.,1.38777878078145E-16));
#21247=DIRECTION('',(1.,0.,-1.38777878078144E-16));
#21248=DIRECTION('',(0.,1.,0.));
#21249=DIRECTION('center_axis',(0.,-1.,0.));
#21250=DIRECTION('ref_axis',(0.,0.,-1.));
#21251=DIRECTION('',(-1.25247756392721E-16,0.,-1.));
#21252=DIRECTION('center_axis',(1.38777878078144E-16,0.,1.));
#21253=DIRECTION('ref_axis',(1.,0.,-1.38777878078145E-16));
#21254=DIRECTION('',(0.,-1.,0.));
#21255=DIRECTION('center_axis',(1.,0.,-1.12538885307499E-16));
#21256=DIRECTION('ref_axis',(1.12538885307499E-16,0.,1.));
#21257=DIRECTION('center_axis',(0.,1.,0.));
#21258=DIRECTION('ref_axis',(0.,0.,1.));
#21259=DIRECTION('',(1.,0.,1.32222068111359E-16));
#21260=DIRECTION('center_axis',(-1.32222068111359E-16,0.,1.));
#21261=DIRECTION('ref_axis',(1.,0.,1.32222068111359E-16));
#21262=DIRECTION('axis',(0.,0.,1.));
#21263=DIRECTION('refdir',(1.,0.,0.));
#21264=DIRECTION('center_axis',(0.,0.,1.));
#21265=DIRECTION('ref_axis',(1.,0.,0.));
#21266=DIRECTION('center_axis',(0.,0.,1.));
#21267=DIRECTION('ref_axis',(1.,0.,0.));
#21268=DIRECTION('',(0.,0.,1.));
#21269=DIRECTION('center_axis',(0.,0.,1.));
#21270=DIRECTION('ref_axis',(1.,0.,0.));
#21271=DIRECTION('center_axis',(0.,0.,-1.));
#21272=DIRECTION('ref_axis',(-1.,0.,0.));
#21273=DIRECTION('center_axis',(0.,0.,1.));
#21274=DIRECTION('ref_axis',(1.,0.,0.));
#21275=DIRECTION('',(0.,0.,-1.));
#21276=DIRECTION('center_axis',(0.,0.,1.));
#21277=DIRECTION('ref_axis',(1.,0.,0.));
#21278=DIRECTION('center_axis',(0.,0.,-1.));
#21279=DIRECTION('ref_axis',(-1.,0.,0.));
#21280=DIRECTION('center_axis',(0.,0.,1.));
#21281=DIRECTION('ref_axis',(1.,0.,0.));
#21282=DIRECTION('',(0.,0.,-1.));
#21283=DIRECTION('center_axis',(0.,0.,1.));
#21284=DIRECTION('ref_axis',(1.,0.,0.));
#21285=DIRECTION('center_axis',(0.,0.,-1.));
#21286=DIRECTION('ref_axis',(-1.,0.,0.));
#21287=DIRECTION('center_axis',(0.,0.,1.));
#21288=DIRECTION('ref_axis',(1.,0.,0.));
#21289=DIRECTION('',(0.,0.,-1.));
#21290=DIRECTION('center_axis',(0.,0.,1.));
#21291=DIRECTION('ref_axis',(1.,0.,0.));
#21292=DIRECTION('center_axis',(0.,0.,-1.));
#21293=DIRECTION('ref_axis',(-1.,0.,0.));
#21294=DIRECTION('center_axis',(0.,0.,1.));
#21295=DIRECTION('ref_axis',(1.,0.,0.));
#21296=DIRECTION('',(0.,0.,-1.));
#21297=DIRECTION('center_axis',(0.,0.,1.));
#21298=DIRECTION('ref_axis',(1.,0.,0.));
#21299=DIRECTION('center_axis',(0.,0.,-1.));
#21300=DIRECTION('ref_axis',(-1.,0.,0.));
#21301=DIRECTION('center_axis',(0.,0.,1.));
#21302=DIRECTION('ref_axis',(1.,0.,0.));
#21303=DIRECTION('',(0.,0.,-1.));
#21304=DIRECTION('center_axis',(0.,0.,1.));
#21305=DIRECTION('ref_axis',(1.,0.,0.));
#21306=DIRECTION('center_axis',(0.,0.,-1.));
#21307=DIRECTION('ref_axis',(-1.,0.,0.));
#21308=DIRECTION('center_axis',(0.,0.,1.));
#21309=DIRECTION('ref_axis',(1.,0.,0.));
#21310=DIRECTION('',(0.,0.,-1.));
#21311=DIRECTION('center_axis',(0.,0.,1.));
#21312=DIRECTION('ref_axis',(1.,0.,0.));
#21313=DIRECTION('center_axis',(0.,0.,-1.));
#21314=DIRECTION('ref_axis',(-1.,0.,0.));
#21315=DIRECTION('center_axis',(0.,0.,1.));
#21316=DIRECTION('ref_axis',(1.,0.,0.));
#21317=DIRECTION('',(0.,0.,-1.));
#21318=DIRECTION('center_axis',(0.,0.,1.));
#21319=DIRECTION('ref_axis',(1.,0.,0.));
#21320=DIRECTION('center_axis',(0.,0.,-1.));
#21321=DIRECTION('ref_axis',(-1.,0.,0.));
#21322=DIRECTION('center_axis',(0.,0.,1.));
#21323=DIRECTION('ref_axis',(1.,0.,0.));
#21324=DIRECTION('',(0.,0.,-1.));
#21325=DIRECTION('center_axis',(0.,0.,1.));
#21326=DIRECTION('ref_axis',(1.,0.,0.));
#21327=DIRECTION('center_axis',(0.,0.,-1.));
#21328=DIRECTION('ref_axis',(-1.,0.,0.));
#21329=DIRECTION('center_axis',(0.,0.,1.));
#21330=DIRECTION('ref_axis',(1.,0.,0.));
#21331=DIRECTION('',(0.,0.,-1.));
#21332=DIRECTION('center_axis',(0.,0.,1.));
#21333=DIRECTION('ref_axis',(1.,0.,0.));
#21334=DIRECTION('center_axis',(0.,0.,-1.));
#21335=DIRECTION('ref_axis',(-1.,0.,0.));
#21336=DIRECTION('center_axis',(0.,0.,1.));
#21337=DIRECTION('ref_axis',(1.,0.,0.));
#21338=DIRECTION('',(0.,0.,-1.));
#21339=DIRECTION('center_axis',(0.,0.,1.));
#21340=DIRECTION('ref_axis',(1.,0.,0.));
#21341=DIRECTION('center_axis',(0.,0.,-1.));
#21342=DIRECTION('ref_axis',(-1.,0.,0.));
#21343=DIRECTION('center_axis',(0.,0.,1.));
#21344=DIRECTION('ref_axis',(1.,0.,0.));
#21345=DIRECTION('',(0.,0.,-1.));
#21346=DIRECTION('center_axis',(0.,0.,1.));
#21347=DIRECTION('ref_axis',(1.,0.,0.));
#21348=DIRECTION('center_axis',(0.,0.,-1.));
#21349=DIRECTION('ref_axis',(-1.,0.,0.));
#21350=DIRECTION('center_axis',(0.,0.,1.));
#21351=DIRECTION('ref_axis',(1.,0.,0.));
#21352=DIRECTION('',(0.,0.,-1.));
#21353=DIRECTION('center_axis',(0.,0.,1.));
#21354=DIRECTION('ref_axis',(1.,0.,0.));
#21355=DIRECTION('center_axis',(0.,0.,-1.));
#21356=DIRECTION('ref_axis',(-1.,0.,0.));
#21357=DIRECTION('center_axis',(0.,0.,1.));
#21358=DIRECTION('ref_axis',(1.,0.,0.));
#21359=DIRECTION('',(0.,0.,-1.));
#21360=DIRECTION('center_axis',(0.,0.,1.));
#21361=DIRECTION('ref_axis',(1.,0.,0.));
#21362=DIRECTION('center_axis',(0.,0.,-1.));
#21363=DIRECTION('ref_axis',(-1.,0.,0.));
#21364=DIRECTION('center_axis',(0.,0.,1.));
#21365=DIRECTION('ref_axis',(1.,0.,0.));
#21366=DIRECTION('',(0.,0.,-1.));
#21367=DIRECTION('center_axis',(0.,0.,1.));
#21368=DIRECTION('ref_axis',(1.,0.,0.));
#21369=DIRECTION('center_axis',(0.,0.,-1.));
#21370=DIRECTION('ref_axis',(-1.,0.,0.));
#21371=DIRECTION('center_axis',(0.,0.,1.));
#21372=DIRECTION('ref_axis',(1.,0.,0.));
#21373=DIRECTION('',(0.,0.,-1.));
#21374=DIRECTION('center_axis',(0.,0.,1.));
#21375=DIRECTION('ref_axis',(1.,0.,0.));
#21376=DIRECTION('center_axis',(0.,0.,-1.));
#21377=DIRECTION('ref_axis',(-1.,0.,0.));
#21378=DIRECTION('center_axis',(0.,0.,1.));
#21379=DIRECTION('ref_axis',(1.,0.,0.));
#21380=DIRECTION('',(0.,0.,1.));
#21381=DIRECTION('center_axis',(0.,0.,1.));
#21382=DIRECTION('ref_axis',(1.,0.,0.));
#21383=DIRECTION('center_axis',(0.,0.,1.));
#21384=DIRECTION('ref_axis',(1.,0.,0.));
#21385=DIRECTION('center_axis',(0.,0.,1.));
#21386=DIRECTION('ref_axis',(1.,0.,0.));
#21387=DIRECTION('center_axis',(0.,0.,1.));
#21388=DIRECTION('ref_axis',(1.,0.,0.));
#21389=DIRECTION('center_axis',(0.,0.,1.));
#21390=DIRECTION('ref_axis',(1.,0.,0.));
#21391=DIRECTION('',(0.,0.,-1.));
#21392=DIRECTION('center_axis',(0.,0.,1.));
#21393=DIRECTION('ref_axis',(1.,0.,0.));
#21394=DIRECTION('center_axis',(0.,0.,1.));
#21395=DIRECTION('ref_axis',(1.,0.,0.));
#21396=DIRECTION('center_axis',(0.,0.,1.));
#21397=DIRECTION('ref_axis',(1.,0.,0.));
#21398=DIRECTION('axis',(0.,0.,1.));
#21399=DIRECTION('refdir',(1.,0.,0.));
#21400=DIRECTION('center_axis',(-3.54454368418083E-15,1.14635476884388E-13,
1.));
#21401=DIRECTION('ref_axis',(1.,0.,4.17966315152979E-15));
#21402=DIRECTION('center_axis',(9.64418253237272E-27,-1.07981213846331E-13,
-1.));
#21403=DIRECTION('ref_axis',(-8.4885105576653E-14,1.,-1.07981213846331E-13));
#21404=DIRECTION('center_axis',(-1.30614473484947E-16,1.,-1.14635476884388E-13));
#21405=DIRECTION('ref_axis',(-1.,-1.30614473485306E-16,-3.13474736364734E-15));
#21406=DIRECTION('center_axis',(1.00515054169548E-26,-1.1518563880486E-13,
-1.));
#21407=DIRECTION('ref_axis',(-8.54871728961371E-14,1.,-1.1518563880486E-13));
#21408=DIRECTION('center_axis',(1.00515054169548E-26,-1.1518563880486E-13,
-1.));
#21409=DIRECTION('ref_axis',(-8.54871728961371E-14,1.,-1.1518563880486E-13));
#21410=DIRECTION('center_axis',(-9.8017643219864E-16,1.15516038958398E-13,
1.));
#21411=DIRECTION('ref_axis',(1.,0.,8.88178419700135E-16));
#21412=DIRECTION('center_axis',(-1.00515054169548E-26,1.1518563880486E-13,
1.));
#21413=DIRECTION('ref_axis',(8.72635297355373E-14,-1.,1.1518563880486E-13));
#21414=DIRECTION('center_axis',(1.38777878078018E-16,-1.,1.15516038958398E-13));
#21415=DIRECTION('ref_axis',(-1.,-1.38777878078146E-16,-1.11022302462517E-15));
#21416=DIRECTION('center_axis',(-1.00515054169548E-26,1.1518563880486E-13,
1.));
#21417=DIRECTION('ref_axis',(-8.72635297355373E-14,1.,-1.1518563880486E-13));
#21418=DIRECTION('center_axis',(-1.00515054169548E-26,1.1518563880486E-13,
1.));
#21419=DIRECTION('ref_axis',(-8.72635297355373E-14,1.,-1.1518563880486E-13));
#21420=DIRECTION('center_axis',(-1.00515054169548E-26,1.1518563880486E-13,
1.));
#21421=DIRECTION('ref_axis',(8.72635297355373E-14,-1.,1.1518563880486E-13));
#21422=DIRECTION('center_axis',(7.85454768979583E-16,1.15103843509475E-13,
1.));
#21423=DIRECTION('ref_axis',(1.,0.,-5.74175948088969E-16));
#21424=DIRECTION('center_axis',(-1.00515054169548E-26,1.1518563880486E-13,
1.));
#21425=DIRECTION('ref_axis',(-8.72635297355373E-14,1.,-1.1518563880486E-13));
#21426=DIRECTION('center_axis',(-1.34572487833435E-16,1.,-1.15103843509475E-13));
#21427=DIRECTION('ref_axis',(-1.,-1.34572487833352E-16,7.17719935111211E-16));
#21428=DIRECTION('center_axis',(-1.00515054169548E-26,1.1518563880486E-13,
1.));
#21429=DIRECTION('ref_axis',(-8.72635297355373E-14,1.,-1.1518563880486E-13));
#21430=DIRECTION('center_axis',(-1.00515054169548E-26,1.1518563880486E-13,
1.));
#21431=DIRECTION('ref_axis',(-8.72635297355373E-14,1.,-1.1518563880486E-13));
#21432=DIRECTION('center_axis',(-1.00515054169548E-26,1.1518563880486E-13,
1.));
#21433=DIRECTION('ref_axis',(-8.72635297355373E-14,1.,-1.1518563880486E-13));
#21434=DIRECTION('center_axis',(2.09517191469308E-15,1.14089507593872E-13,
1.));
#21435=DIRECTION('ref_axis',(1.,0.,-2.18628534080032E-15));
#21436=DIRECTION('center_axis',(-1.00515054169548E-26,1.1518563880486E-13,
1.));
#21437=DIRECTION('ref_axis',(8.72635297355373E-14,-1.,1.1518563880486E-13));
#21438=DIRECTION('center_axis',(-1.13869028166891E-16,1.,-1.14089507593872E-13));
#21439=DIRECTION('ref_axis',(-1.,-1.13869028166684E-16,1.82190445066694E-15));
#21440=DIRECTION('center_axis',(1.00515054169548E-26,-1.1518563880486E-13,
-1.));
#21441=DIRECTION('ref_axis',(8.72635297355373E-14,-1.,1.1518563880486E-13));
#21442=DIRECTION('center_axis',(1.00515054169548E-26,-1.1518563880486E-13,
-1.));
#21443=DIRECTION('ref_axis',(8.72635297355373E-14,-1.,1.1518563880486E-13));
#21444=DIRECTION('center_axis',(-1.00515054169548E-26,1.1518563880486E-13,
1.));
#21445=DIRECTION('ref_axis',(8.72635297355373E-14,-1.,1.1518563880486E-13));
#21446=DIRECTION('center_axis',(-1.00515054169548E-26,1.1518563880486E-13,
1.));
#21447=DIRECTION('ref_axis',(-8.72635297355373E-14,1.,-1.1518563880486E-13));
#21448=DIRECTION('center_axis',(2.90839696048352E-15,1.12070336644323E-13,
1.));
#21449=DIRECTION('ref_axis',(1.,8.67992546525122E-14,-3.22973970800046E-15));
#21450=DIRECTION('',(-1.00515054169548E-26,1.1518563880486E-13,1.));
#21451=DIRECTION('center_axis',(-8.92186509493858E-16,1.14732495036932E-13,
1.));
#21452=DIRECTION('ref_axis',(8.6535488860372E-14,-1.,1.14978733604816E-13));
#21453=DIRECTION('center_axis',(1.00515054169548E-26,-1.1518563880486E-13,
-1.));
#21454=DIRECTION('ref_axis',(8.72635297355373E-14,-1.,1.1518563880486E-13));
#21455=DIRECTION('',(8.21476117669779E-14,-0.94269689858097,0.333650352024124));
#21456=DIRECTION('center_axis',(-1.00515054169548E-26,1.1518563880486E-13,
1.));
#21457=DIRECTION('ref_axis',(-8.72635297355373E-14,1.,-1.1518563880486E-13));
#21458=DIRECTION('',(4.00335205749406E-14,-0.458122847290751,0.888888888888941));
#21459=DIRECTION('center_axis',(-1.00489519728121E-26,1.15107923193136E-13,
1.));
#21460=DIRECTION('ref_axis',(-8.71826535283427E-14,1.,-1.15107923193136E-13));
#21461=DIRECTION('center_axis',(1.00515054169548E-26,-1.1518563880486E-13,
-1.));
#21462=DIRECTION('ref_axis',(8.72635297355373E-14,-1.,1.1518563880486E-13));
#21463=DIRECTION('',(7.26903855506451E-14,-0.834169119969402,0.551508730021088));
#21464=DIRECTION('center_axis',(1.00515054169548E-26,-1.1518563880486E-13,
-1.));
#21465=DIRECTION('ref_axis',(8.72635297355373E-14,-1.,1.1518563880486E-13));
#21466=DIRECTION('',(8.70424333714333E-14,-0.998868137724432,0.0475651494155674));
#21467=DIRECTION('center_axis',(-1.00515054169548E-26,1.1518563880486E-13,
1.));
#21468=DIRECTION('ref_axis',(-8.72635297355373E-14,1.,-1.1518563880486E-13));
#21469=DIRECTION('center_axis',(1.00515054169548E-26,-1.1518563880486E-13,
-1.));
#21470=DIRECTION('ref_axis',(8.72635297355373E-14,-1.,1.1518563880486E-13));
#21471=DIRECTION('center_axis',(-8.72635297355373E-14,1.,-1.1518563880486E-13));
#21472=DIRECTION('ref_axis',(1.0285184916872E-26,-1.1518563880486E-13,-1.));
#21473=DIRECTION('center_axis',(8.72635297355373E-14,-1.,1.1518563880486E-13));
#21474=DIRECTION('ref_axis',(-1.86517468136924E-14,-1.15185638804862E-13,
-1.));
#21475=DIRECTION('center_axis',(8.72635297355373E-14,-1.,1.1518563880486E-13));
#21476=DIRECTION('ref_axis',(-1.86517468136924E-14,-1.15185638804862E-13,
-1.));
#21477=DIRECTION('',(8.55449136515341E-14,-0.980580675690943,-0.196116135138071));
#21478=DIRECTION('center_axis',(-9.43689570926916E-14,1.,1.83186799062301E-13));
#21479=DIRECTION('ref_axis',(6.03740488023232E-15,-1.77635683939193E-13,
1.));
#21480=DIRECTION('center_axis',(8.72635297355373E-14,-1.,1.1518563880486E-13));
#21481=DIRECTION('ref_axis',(-1.06184991926244E-26,1.1518563880486E-13,
1.));
#21482=DIRECTION('',(7.81056416479254E-14,-0.894427190999967,-0.447213595499855));
#21483=DIRECTION('center_axis',(8.88178419730948E-14,-1.,7.10542735786571E-13));
#21484=DIRECTION('ref_axis',(7.57155095484643E-15,7.10542735786545E-13,
1.));
#21485=DIRECTION('center_axis',(8.72635297355373E-14,-1.,1.1518563880486E-13));
#21486=DIRECTION('ref_axis',(-1.00515054169548E-26,1.1518563880486E-13,
1.));
#21487=DIRECTION('center_axis',(8.72635297355373E-14,-1.,1.1518563880486E-13));
#21488=DIRECTION('ref_axis',(-9.82963828734632E-27,1.1518563880486E-13,
1.));
#21489=DIRECTION('',(7.81056416599154E-14,-0.894427191137758,-0.447213595224274));
#21490=DIRECTION('center_axis',(-8.72635297355373E-14,1.,-1.1518563880486E-13));
#21491=DIRECTION('ref_axis',(-9.82963828734632E-27,1.1518563880486E-13,
1.));
#21492=DIRECTION('center_axis',(-8.72635297355373E-14,1.,-1.1518563880486E-13));
#21493=DIRECTION('ref_axis',(1.00515054169548E-26,-1.1518563880486E-13,
-1.));
#21494=DIRECTION('center_axis',(1.,8.72635297355373E-14,0.));
#21495=DIRECTION('ref_axis',(8.72635297355373E-14,-1.,1.1518563880486E-13));
#21496=DIRECTION('',(4.36317648660981E-14,-0.499999999980857,-0.866025403795491));
#21497=DIRECTION('',(-4.36317648660809E-14,0.49999999998066,-0.866025403795605));
#21498=DIRECTION('',(-8.72635297355373E-14,1.,-1.1518563880486E-13));
#21499=DIRECTION('',(-4.36317648660983E-14,0.499999999980859,0.86602540379549));
#21500=DIRECTION('',(4.36317648660808E-14,-0.499999999980657,0.866025403795606));
#21501=DIRECTION('',(8.72635297355373E-14,-1.,1.1518563880486E-13));
#21502=DIRECTION('center_axis',(7.55724335758485E-14,-0.866025403795606,
-0.499999999980658));
#21503=DIRECTION('ref_axis',(4.36317648660808E-14,-0.499999999980658,0.866025403795606));
#21504=DIRECTION('',(1.,8.72635297355373E-14,0.));
#21505=DIRECTION('',(-1.,-8.72635297355373E-14,0.));
#21506=DIRECTION('',(4.36317648660808E-14,-0.499999999980658,0.866025403795606));
#21507=DIRECTION('center_axis',(7.55724335758385E-14,-0.86602540379549,
0.499999999980858));
#21508=DIRECTION('ref_axis',(-4.36317648660983E-14,0.499999999980858,0.86602540379549));
#21509=DIRECTION('',(-1.,-8.72635297355373E-14,0.));
#21510=DIRECTION('',(-4.36317648660983E-14,0.499999999980858,0.86602540379549));
#21511=DIRECTION('center_axis',(-1.00515054169548E-26,1.1518563880486E-13,
1.));
#21512=DIRECTION('ref_axis',(-8.72635297355373E-14,1.,-1.1518563880486E-13));
#21513=DIRECTION('',(-1.,-8.72635297355373E-14,0.));
#21514=DIRECTION('',(0.133254699246628,0.991081825647454,-1.14158393195087E-13));
#21515=DIRECTION('',(-8.72635297355373E-14,1.,-1.1518563880486E-13));
#21516=DIRECTION('center_axis',(-7.55724335758485E-14,0.866025403795606,
0.499999999980658));
#21517=DIRECTION('ref_axis',(-4.36317648660808E-14,0.499999999980658,-0.866025403795606));
#21518=DIRECTION('',(-1.,-8.72635297355373E-14,0.));
#21519=DIRECTION('',(0.0670754893014342,0.498873951679673,-0.864075030926412));
#21520=DIRECTION('center_axis',(-7.55724335758385E-14,0.86602540379549,
-0.499999999980858));
#21521=DIRECTION('ref_axis',(4.36317648660983E-14,-0.499999999980858,-0.86602540379549));
#21522=DIRECTION('',(-1.,-8.72635297355373E-14,0.));
#21523=DIRECTION('',(-0.0670754893014346,-0.498873951679872,-0.864075030926297));
#21524=DIRECTION('center_axis',(1.00515054169548E-26,-1.1518563880486E-13,
-1.));
#21525=DIRECTION('ref_axis',(8.72635297355373E-14,-1.,1.1518563880486E-13));
#21526=DIRECTION('',(-0.133254699246661,-0.99108182564745,1.14158393195087E-13));
#21527=DIRECTION('',(8.72635297355373E-14,-1.,1.1518563880486E-13));
#21528=DIRECTION('center_axis',(-1.,-8.72635297355373E-14,0.));
#21529=DIRECTION('ref_axis',(-8.72635297355373E-14,1.,-1.1518563880486E-13));
#21530=DIRECTION('',(1.00515054169548E-26,-1.1518563880486E-13,-1.));
#21531=DIRECTION('center_axis',(-0.991081825647454,0.133254699246628,-1.53490276564824E-14));
#21532=DIRECTION('ref_axis',(0.133254699246628,0.991081825647454,-1.14158393195087E-13));
#21533=DIRECTION('',(-0.585068654159542,-0.386550578869277,-0.712932899995342));
#21534=DIRECTION('',(-0.35948002755914,-0.539309464528629,-0.761524399645818));
#21535=DIRECTION('',(-0.379976420578218,-0.590823050535381,-0.711720480779239));
#21536=DIRECTION('center_axis',(4.08987016959577E-16,-1.15239837533439E-13,
-1.));
#21537=DIRECTION('ref_axis',(-1.,0.,-3.13169680337459E-16));
#21538=DIRECTION('center_axis',(1.00515054169548E-26,-1.1518563880486E-13,
-1.));
#21539=DIRECTION('ref_axis',(8.72635297355373E-14,-1.,1.1518563880486E-13));
#21540=DIRECTION('center_axis',(-1.22464679914813E-16,-1.,1.15239837533439E-13));
#21541=DIRECTION('ref_axis',(1.,-1.22464679914768E-16,3.91462100421824E-16));
#21542=DIRECTION('center_axis',(1.00515054169548E-26,-1.1518563880486E-13,
-1.));
#21543=DIRECTION('ref_axis',(-8.72635297355373E-14,1.,-1.1518563880486E-13));
#21544=DIRECTION('center_axis',(1.00515054169548E-26,-1.1518563880486E-13,
-1.));
#21545=DIRECTION('ref_axis',(-8.72635297355373E-14,1.,-1.1518563880486E-13));
#21546=DIRECTION('center_axis',(-8.72635297355373E-14,1.,-1.1518563880486E-13));
#21547=DIRECTION('ref_axis',(4.48527684827171E-30,-1.1518563880486E-13,
-1.));
#21548=DIRECTION('center_axis',(-8.72635297355373E-14,1.,-1.1518563880486E-13));
#21549=DIRECTION('ref_axis',(4.48527684827171E-30,-1.1518563880486E-13,
-1.));
#21550=DIRECTION('',(-8.72635297355373E-14,1.,-1.1518563880486E-13));
#21551=DIRECTION('center_axis',(8.72635297355373E-14,-1.,1.1518563880486E-13));
#21552=DIRECTION('ref_axis',(4.48527684827171E-30,-1.1518563880486E-13,
-1.));
#21553=DIRECTION('center_axis',(-8.72635297355373E-14,1.,-1.1518563880486E-13));
#21554=DIRECTION('ref_axis',(4.48527684826454E-30,-1.1518563880486E-13,
-1.));
#21555=DIRECTION('center_axis',(-8.72635297355373E-14,1.,-1.1518563880486E-13));
#21556=DIRECTION('ref_axis',(4.48527684826454E-30,-1.1518563880486E-13,
-1.));
#21557=DIRECTION('',(-8.72635297355373E-14,1.,-1.1518563880486E-13));
#21558=DIRECTION('center_axis',(8.72635297355373E-14,-1.,1.1518563880486E-13));
#21559=DIRECTION('ref_axis',(4.48527684826023E-30,-1.1518563880486E-13,
-1.));
#21560=DIRECTION('center_axis',(-8.72635297355373E-14,1.,-1.1518563880486E-13));
#21561=DIRECTION('ref_axis',(4.48527684827171E-30,-1.1518563880486E-13,
-1.));
#21562=DIRECTION('center_axis',(-8.72635297355373E-14,1.,-1.1518563880486E-13));
#21563=DIRECTION('ref_axis',(4.48527684827171E-30,-1.1518563880486E-13,
-1.));
#21564=DIRECTION('',(-8.72635297355373E-14,1.,-1.1518563880486E-13));
#21565=DIRECTION('center_axis',(8.72635297355373E-14,-1.,1.1518563880486E-13));
#21566=DIRECTION('ref_axis',(4.48527684827171E-30,-1.1518563880486E-13,
-1.));
#21567=DIRECTION('center_axis',(-8.72635297355373E-14,1.,-1.1518563880486E-13));
#21568=DIRECTION('ref_axis',(4.48527684826454E-30,-1.1518563880486E-13,
-1.));
#21569=DIRECTION('center_axis',(-8.72635297355373E-14,1.,-1.1518563880486E-13));
#21570=DIRECTION('ref_axis',(4.48527684826454E-30,-1.1518563880486E-13,
-1.));
#21571=DIRECTION('',(-8.72635297355373E-14,1.,-1.1518563880486E-13));
#21572=DIRECTION('center_axis',(8.72635297355373E-14,-1.,1.1518563880486E-13));
#21573=DIRECTION('ref_axis',(4.48527684826023E-30,-1.1518563880486E-13,
-1.));
#21574=DIRECTION('center_axis',(1.,8.72635297355373E-14,0.));
#21575=DIRECTION('ref_axis',(8.72635297355373E-14,-1.,1.1498738469332E-13));
#21576=DIRECTION('center_axis',(1.,8.72635297355373E-14,0.));
#21577=DIRECTION('ref_axis',(8.72635297355373E-14,-1.,1.1498738469332E-13));
#21578=DIRECTION('center_axis',(0.988934829411352,0.148350608954393,-5.96763239577493E-15));
#21579=DIRECTION('ref_axis',(0.148350608954393,-0.988934829411352,-6.02957470936365E-12));
#21580=DIRECTION('',(-1.,-8.72635297355373E-14,0.));
#21581=DIRECTION('center_axis',(1.,8.72635297355373E-14,0.));
#21582=DIRECTION('ref_axis',(8.72635297355373E-14,-1.,1.1498738469332E-13));
#21583=DIRECTION('center_axis',(0.988934829411352,0.148350608954393,-5.96763239577493E-15));
#21584=DIRECTION('ref_axis',(0.148350608954393,-0.988934829411352,-6.02957470936365E-12));
#21585=DIRECTION('center_axis',(1.00515054169548E-26,-1.1518563880486E-13,
-1.));
#21586=DIRECTION('ref_axis',(8.73039014818873E-14,-1.,1.1518563880486E-13));
#21587=DIRECTION('center_axis',(1.00515054169548E-26,-1.1518563880486E-13,
-1.));
#21588=DIRECTION('ref_axis',(8.73039014818873E-14,-1.,1.1518563880486E-13));
#21589=DIRECTION('center_axis',(-1.00515054169548E-26,1.1518563880486E-13,
1.));
#21590=DIRECTION('ref_axis',(8.73039014818873E-14,-1.,1.1518563880486E-13));
#21591=DIRECTION('center_axis',(1.00515054169548E-26,-1.1518563880486E-13,
-1.));
#21592=DIRECTION('ref_axis',(8.72635297355373E-14,-1.,1.1518563880486E-13));
#21593=DIRECTION('center_axis',(1.00515054169548E-26,-1.1518563880486E-13,
-1.));
#21594=DIRECTION('ref_axis',(8.72635297355373E-14,-1.,1.1518563880486E-13));
#21595=DIRECTION('center_axis',(1.00515054169548E-26,-1.1518563880486E-13,
-1.));
#21596=DIRECTION('ref_axis',(8.72635297355373E-14,-1.,1.1518563880486E-13));
#21597=DIRECTION('center_axis',(-1.00515054169548E-26,1.1518563880486E-13,
1.));
#21598=DIRECTION('ref_axis',(8.72635297355373E-14,-1.,1.1518563880486E-13));
#21599=DIRECTION('center_axis',(-1.00515054169548E-26,1.1518563880486E-13,
1.));
#21600=DIRECTION('ref_axis',(8.72635297355373E-14,-1.,1.1518563880486E-13));
#21601=DIRECTION('center_axis',(1.00515054169548E-26,-1.1518563880486E-13,
-1.));
#21602=DIRECTION('ref_axis',(8.72092802013795E-14,-1.,1.1518563880486E-13));
#21603=DIRECTION('center_axis',(1.00515054169548E-26,-1.1518563880486E-13,
-1.));
#21604=DIRECTION('ref_axis',(8.72092802013795E-14,-1.,1.1518563880486E-13));
#21605=DIRECTION('center_axis',(-1.00515054169548E-26,1.1518563880486E-13,
1.));
#21606=DIRECTION('ref_axis',(8.72092802013795E-14,-1.,1.1518563880486E-13));
#21607=DIRECTION('center_axis',(1.00515054169548E-26,-1.1518563880486E-13,
-1.));
#21608=DIRECTION('ref_axis',(8.72318090776909E-14,-1.,1.1518563880486E-13));
#21609=DIRECTION('center_axis',(-1.00515054169548E-26,1.1518563880486E-13,
1.));
#21610=DIRECTION('ref_axis',(8.72318090776909E-14,-1.,1.1518563880486E-13));
#21611=DIRECTION('',(-1.00515054169548E-26,1.1518563880486E-13,1.));
#21612=DIRECTION('center_axis',(1.00515054169548E-26,-1.1518563880486E-13,
-1.));
#21613=DIRECTION('ref_axis',(8.72318090776909E-14,-1.,1.1518563880486E-13));
#21614=DIRECTION('center_axis',(1.,8.72635297355373E-14,0.));
#21615=DIRECTION('ref_axis',(8.72635297355373E-14,-1.,1.1498738469332E-13));
#21616=DIRECTION('center_axis',(-1.,-8.72635297355373E-14,0.));
#21617=DIRECTION('ref_axis',(8.72635297355373E-14,-1.,1.1498738469332E-13));
#21618=DIRECTION('',(-1.,-8.72635297355373E-14,0.));
#21619=DIRECTION('center_axis',(-1.,-8.72635297355373E-14,0.));
#21620=DIRECTION('ref_axis',(8.72635297355373E-14,-1.,1.1498738469332E-13));
#21621=DIRECTION('center_axis',(-1.,-8.72635297355373E-14,0.));
#21622=DIRECTION('ref_axis',(8.72635297355373E-14,-1.,1.16969925808722E-13));
#21623=DIRECTION('center_axis',(-1.,-8.72635297355373E-14,0.));
#21624=DIRECTION('ref_axis',(8.72635297355373E-14,-1.,1.18952466924124E-13));
#21625=DIRECTION('center_axis',(1.,8.72635297355373E-14,0.));
#21626=DIRECTION('ref_axis',(8.72635297355373E-14,-1.,1.1498738469332E-13));
#21627=DIRECTION('center_axis',(1.,8.72635297355373E-14,0.));
#21628=DIRECTION('ref_axis',(8.72635297355373E-14,-1.,1.1498738469332E-13));
#21629=DIRECTION('center_axis',(0.991081825647456,-0.133254699246617,2.83668489712038E-13));
#21630=DIRECTION('ref_axis',(0.133254699246616,0.991081825647456,-1.1265578716007E-10));
#21631=DIRECTION('center_axis',(-1.,-8.72635297355373E-14,0.));
#21632=DIRECTION('ref_axis',(8.72635297355373E-14,-1.,1.1498738469332E-13));
#21633=DIRECTION('',(-1.,-8.72635297355373E-14,0.));
#21634=DIRECTION('center_axis',(1.,8.72635297355373E-14,0.));
#21635=DIRECTION('ref_axis',(8.72635297355373E-14,-1.,1.1498738469332E-13));
#21636=DIRECTION('center_axis',(-1.,-8.72635297355373E-14,0.));
#21637=DIRECTION('ref_axis',(8.72635297355373E-14,-1.,1.1498738469332E-13));
#21638=DIRECTION('center_axis',(0.991081825647462,-0.133254699246573,-3.75601193874917E-13));
#21639=DIRECTION('ref_axis',(0.133254699246573,0.991081825647462,4.6681475548608E-11));
#21640=DIRECTION('center_axis',(1.00515054169548E-26,-1.1518563880486E-13,
-1.));
#21641=DIRECTION('ref_axis',(8.72635297355373E-14,-1.,1.1518563880486E-13));
#21642=DIRECTION('center_axis',(-1.00515054169548E-26,1.1518563880486E-13,
1.));
#21643=DIRECTION('ref_axis',(8.72635297355373E-14,-1.,1.1518563880486E-13));
#21644=DIRECTION('',(-1.00515054169548E-26,1.1518563880486E-13,1.));
#21645=DIRECTION('center_axis',(-1.00515054169548E-26,1.1518563880486E-13,
1.));
#21646=DIRECTION('ref_axis',(8.72635297355373E-14,-1.,1.1518563880486E-13));
#21647=DIRECTION('center_axis',(1.00515054169548E-26,-1.1518563880486E-13,
-1.));
#21648=DIRECTION('ref_axis',(8.72635297355373E-14,-1.,1.1518563880486E-13));
#21649=DIRECTION('center_axis',(-1.00515054169548E-26,1.1518563880486E-13,
1.));
#21650=DIRECTION('ref_axis',(8.72635297355373E-14,-1.,1.1518563880486E-13));
#21651=DIRECTION('',(-1.00515054169548E-26,1.1518563880486E-13,1.));
#21652=DIRECTION('center_axis',(1.00515054169548E-26,-1.1518563880486E-13,
-1.));
#21653=DIRECTION('ref_axis',(8.72635297355373E-14,-1.,1.1518563880486E-13));
#21654=DIRECTION('center_axis',(9.74874922969709E-27,-1.11716191852906E-13,
-1.));
#21655=DIRECTION('ref_axis',(8.73144149574993E-14,-1.,1.11716191852906E-13));
#21656=DIRECTION('',(-9.74874922969709E-27,1.11716191852906E-13,1.));
#21657=DIRECTION('',(9.74874922969709E-27,-1.11716191852906E-13,-1.));
#21658=DIRECTION('center_axis',(9.74874922969709E-27,-1.11716191852906E-13,
-1.));
#21659=DIRECTION('ref_axis',(8.73144149574993E-14,-1.,1.11716191852906E-13));
#21660=DIRECTION('',(-9.74874922969709E-27,1.11716191852906E-13,1.));
#21661=DIRECTION('',(9.74874922969709E-27,-1.11716191852906E-13,-1.));
#21662=DIRECTION('center_axis',(9.74874922969709E-27,-1.11716191852906E-13,
-1.));
#21663=DIRECTION('ref_axis',(8.73144149574993E-14,-1.,1.11716191852906E-13));
#21664=DIRECTION('center_axis',(-0.86602540378444,-1.44241112198798E-13,
-0.499999999999998));
#21665=DIRECTION('ref_axis',(0.499999999999998,-5.6498411616905E-12,-0.86602540378444));
#21666=DIRECTION('',(-9.74874922969709E-27,1.11716191852906E-13,1.));
#21667=DIRECTION('center_axis',(-0.866025403784441,-1.99589445949051E-13,
0.499999999999995));
#21668=DIRECTION('ref_axis',(0.499999999999995,-1.38913863763611E-11,0.866025403784441));
#21669=DIRECTION('',(9.74874922969709E-27,-1.11716191852906E-13,-1.));
#21670=DIRECTION('center_axis',(9.74874922969709E-27,-1.11716191852906E-13,
-1.));
#21671=DIRECTION('ref_axis',(8.73144149574993E-14,-1.,1.11716191852906E-13));
#21672=DIRECTION('',(-9.74874922969709E-27,1.11716191852906E-13,1.));
#21673=DIRECTION('center_axis',(-9.74874922969709E-27,1.11716191852906E-13,
1.));
#21674=DIRECTION('ref_axis',(8.38449680055457E-14,-1.,1.11716191852906E-13));
#21675=DIRECTION('',(9.74874922969709E-27,-1.11716191852906E-13,-1.));
#21676=DIRECTION('center_axis',(9.74874922969709E-27,-1.11716191852906E-13,
-1.));
#21677=DIRECTION('ref_axis',(8.73144149574993E-14,-1.,1.11716191852906E-13));
#21678=DIRECTION('',(-9.74874922969709E-27,1.11716191852906E-13,1.));
#21679=DIRECTION('',(9.74874922969709E-27,-1.11716191852906E-13,-1.));
#21680=DIRECTION('center_axis',(-1.00515054169548E-26,1.1518563880486E-13,
1.));
#21681=DIRECTION('ref_axis',(0.923879532511253,0.382683432365171,-4.40796356170093E-14));
#21682=DIRECTION('center_axis',(-1.00515054169548E-26,1.1518563880486E-13,
1.));
#21683=DIRECTION('ref_axis',(-8.72635297355373E-14,1.,-1.1518563880486E-13));
#21684=DIRECTION('center_axis',(-1.00515054169548E-26,1.1518563880486E-13,
1.));
#21685=DIRECTION('ref_axis',(-8.72635297355373E-14,1.,-1.1518563880486E-13));
#21686=DIRECTION('',(-1.00515054169548E-26,1.1518563880486E-13,1.));
#21687=DIRECTION('center_axis',(1.00515054169548E-26,-1.1518563880486E-13,
-1.));
#21688=DIRECTION('ref_axis',(-8.90398865749375E-14,1.,-1.1518563880486E-13));
#21689=DIRECTION('',(-1.00515054169548E-26,1.1518563880486E-13,1.));
#21690=DIRECTION('center_axis',(-1.00515054169548E-26,1.1518563880486E-13,
1.));
#21691=DIRECTION('ref_axis',(-8.72635297355372E-14,1.,-1.1518563880486E-13));
#21692=DIRECTION('center_axis',(1.00515054169548E-26,-1.1518563880486E-13,
-1.));
#21693=DIRECTION('ref_axis',(-8.72635297355372E-14,1.,-1.1518563880486E-13));
#21694=DIRECTION('',(-1.00515054169548E-26,1.1518563880486E-13,1.));
#21695=DIRECTION('center_axis',(1.00515054169548E-26,-1.1518563880486E-13,
-1.));
#21696=DIRECTION('ref_axis',(-8.72635297355372E-14,1.,-1.1518563880486E-13));
#21697=DIRECTION('center_axis',(-1.00515054169548E-26,1.1518563880486E-13,
1.));
#21698=DIRECTION('ref_axis',(-8.63506796930677E-14,1.,-1.1518563880486E-13));
#21699=DIRECTION('center_axis',(1.00515054169548E-26,-1.1518563880486E-13,
-1.));
#21700=DIRECTION('ref_axis',(-8.63506796930677E-14,1.,-1.1518563880486E-13));
#21701=DIRECTION('',(-1.00515054169548E-26,1.1518563880486E-13,1.));
#21702=DIRECTION('center_axis',(1.00515054169548E-26,-1.1518563880486E-13,
-1.));
#21703=DIRECTION('ref_axis',(-8.63506796930677E-14,1.,-1.1518563880486E-13));
#21704=DIRECTION('center_axis',(-1.00515054169548E-26,1.1518563880486E-13,
1.));
#21705=DIRECTION('ref_axis',(-8.72635297355373E-14,1.,-1.1518563880486E-13));
#21706=DIRECTION('center_axis',(1.00515054169548E-26,-1.1518563880486E-13,
-1.));
#21707=DIRECTION('ref_axis',(-8.72635297355373E-14,1.,-1.1518563880486E-13));
#21708=DIRECTION('',(-1.00515054169548E-26,1.1518563880486E-13,1.));
#21709=DIRECTION('center_axis',(1.00515054169548E-26,-1.1518563880486E-13,
-1.));
#21710=DIRECTION('ref_axis',(-8.72635297355373E-14,1.,-1.1518563880486E-13));
#21711=DIRECTION('center_axis',(-1.00515054169548E-26,1.1518563880486E-13,
1.));
#21712=DIRECTION('ref_axis',(-8.63506796930677E-14,1.,-1.1518563880486E-13));
#21713=DIRECTION('center_axis',(1.00515054169548E-26,-1.1518563880486E-13,
-1.));
#21714=DIRECTION('ref_axis',(-8.63506796930677E-14,1.,-1.1518563880486E-13));
#21715=DIRECTION('',(-1.00515054169548E-26,1.1518563880486E-13,1.));
#21716=DIRECTION('center_axis',(1.00515054169548E-26,-1.1518563880486E-13,
-1.));
#21717=DIRECTION('ref_axis',(-8.63506796930677E-14,1.,-1.1518563880486E-13));
#21718=DIRECTION('center_axis',(1.00515054169548E-26,-1.1518563880486E-13,
-1.));
#21719=DIRECTION('ref_axis',(8.72635297355373E-14,-1.,1.1518563880486E-13));
#21720=DIRECTION('center_axis',(1.00515054169548E-26,-1.1518563880486E-13,
-1.));
#21721=DIRECTION('ref_axis',(8.72635297355373E-14,-1.,1.1518563880486E-13));
#21722=DIRECTION('',(-1.00515054169548E-26,1.1518563880486E-13,1.));
#21723=DIRECTION('center_axis',(1.00515054169548E-26,-1.1518563880486E-13,
-1.));
#21724=DIRECTION('ref_axis',(8.72635297355373E-14,-1.,1.1518563880486E-13));
#21725=DIRECTION('center_axis',(9.74874922969709E-27,-1.11716191852906E-13,
-1.));
#21726=DIRECTION('ref_axis',(8.73144149574993E-14,-1.,1.11716191852906E-13));
#21727=DIRECTION('center_axis',(9.74874922969709E-27,-1.11716191852906E-13,
-1.));
#21728=DIRECTION('ref_axis',(8.73144149574993E-14,-1.,1.11716191852906E-13));
#21729=DIRECTION('',(-9.74874922969709E-27,1.11716191852906E-13,1.));
#21730=DIRECTION('',(9.74874922969709E-27,-1.11716191852906E-13,-1.));
#21731=DIRECTION('center_axis',(-8.72635297355373E-14,1.,-1.11716191852906E-13));
#21732=DIRECTION('ref_axis',(-6.05512374515382E-29,-1.11716191852906E-13,
-1.));
#21733=DIRECTION('center_axis',(-8.72635297355373E-14,1.,-1.11716191852906E-13));
#21734=DIRECTION('ref_axis',(-6.05512374515382E-29,-1.11716191852906E-13,
-1.));
#21735=DIRECTION('',(8.87753855036761E-14,-1.,1.14312768470149E-13));
#21736=DIRECTION('',(-8.57516739673986E-14,1.,-1.14312768470149E-13));
#21737=DIRECTION('center_axis',(9.74874922969709E-27,-1.11716191852906E-13,
-1.));
#21738=DIRECTION('ref_axis',(8.73144149574993E-14,-1.,1.11716191852906E-13));
#21739=DIRECTION('center_axis',(0.86602540378444,1.19740931593546E-14,-0.499999999999999));
#21740=DIRECTION('ref_axis',(0.499999999999998,4.90026582553221E-12,0.86602540378444));
#21741=DIRECTION('',(-9.74874922969709E-27,1.11716191852906E-13,1.));
#21742=DIRECTION('center_axis',(0.866025403784415,4.89441057888314E-13,
0.500000000000041));
#21743=DIRECTION('ref_axis',(0.500000000000041,-6.4989672014377E-12,-0.866025403784415));
#21744=DIRECTION('',(9.74874922969709E-27,-1.11716191852906E-13,-1.));
#21745=DIRECTION('center_axis',(-1.81408990941771E-16,-1.1518563880486E-13,
-1.));
#21746=DIRECTION('ref_axis',(-1.,-8.72577246478268E-14,1.81408990951822E-16));
#21747=DIRECTION('center_axis',(-1.00515054169548E-26,1.1518563880486E-13,
1.));
#21748=DIRECTION('ref_axis',(8.19344592173366E-14,-1.,1.1518563880486E-13));
#21749=DIRECTION('center_axis',(-1.00515054169548E-26,1.1518563880486E-13,
1.));
#21750=DIRECTION('ref_axis',(8.01581023779363E-14,-1.,1.1518563880486E-13));
#21751=DIRECTION('center_axis',(-1.00515054169548E-26,1.1518563880486E-13,
1.));
#21752=DIRECTION('ref_axis',(8.72635297355373E-14,-1.,1.1518563880486E-13));
#21753=DIRECTION('center_axis',(-1.00515054169548E-26,1.1518563880486E-13,
1.));
#21754=DIRECTION('ref_axis',(8.63753513158372E-14,-1.,1.1518563880486E-13));
#21755=DIRECTION('center_axis',(-1.00515054169548E-26,1.1518563880486E-13,
1.));
#21756=DIRECTION('ref_axis',(8.72635297355373E-14,-1.,1.1518563880486E-13));
#21757=DIRECTION('',(-0.970295726275999,-5.66810422692838E-14,0.241921895599659));
#21758=DIRECTION('center_axis',(-1.00515054169548E-26,1.1518563880486E-13,
1.));
#21759=DIRECTION('ref_axis',(8.72635297355373E-14,-1.,1.1518563880486E-13));
#21760=DIRECTION('center_axis',(-1.00515054169548E-26,1.1518563880486E-13,
1.));
#21761=DIRECTION('ref_axis',(8.01581023779363E-14,-1.,1.1518563880486E-13));
#21762=DIRECTION('center_axis',(-1.00515054169548E-26,1.1518563880486E-13,
1.));
#21763=DIRECTION('ref_axis',(8.45989944764369E-14,-1.,1.1518563880486E-13));
#21764=DIRECTION('center_axis',(-1.00515054169548E-26,1.1518563880486E-13,
1.));
#21765=DIRECTION('ref_axis',(9.79216707719388E-14,-1.,1.1518563880486E-13));
#21766=DIRECTION('center_axis',(0.868162779192246,0.38268343239671,0.315985410097158));
#21767=DIRECTION('ref_axis',(0.403349423721025,-0.915046032931632,1.06907841467309E-13));
#21768=DIRECTION('center_axis',(-0.868162779195909,-0.359604797490725,-0.342020143325639));
#21769=DIRECTION('ref_axis',(0.0151045167327983,0.669702936743006,-0.742475474404415));
#21770=DIRECTION('center_axis',(-0.868162779192246,-0.38268343239671,-0.315985410097158));
#21771=DIRECTION('ref_axis',(0.403349423721026,-0.915046032931631,1.02974997442446E-13));
#21772=DIRECTION('',(-0.868162779192246,-0.38268343239671,-0.315985410097158));
#21773=DIRECTION('center_axis',(0.868162779192246,0.38268343239671,0.315985410097158));
#21774=DIRECTION('ref_axis',(0.403349423721025,-0.915046032931632,1.06907841467309E-13));
#21775=DIRECTION('center_axis',(0.868162779192246,0.38268343239671,0.315985410097158));
#21776=DIRECTION('ref_axis',(0.403349423721025,-0.915046032931632,1.06907841467309E-13));
#21777=DIRECTION('center_axis',(-0.868162779192246,-0.38268343239671,-0.315985410097158));
#21778=DIRECTION('ref_axis',(0.403349423721026,-0.915046032931631,1.02974997442446E-13));
#21779=DIRECTION('center_axis',(9.74874922969709E-27,-1.11716191852906E-13,
-1.));
#21780=DIRECTION('ref_axis',(8.73144149574993E-14,-1.,1.11716191852906E-13));
#21781=DIRECTION('center_axis',(9.74874922969709E-27,-1.11716191852906E-13,
-1.));
#21782=DIRECTION('ref_axis',(8.73144149574993E-14,-1.,1.11716191852906E-13));
#21783=DIRECTION('',(-9.74874922969709E-27,1.11716191852906E-13,1.));
#21784=DIRECTION('center_axis',(-9.74874922969709E-27,1.11716191852906E-13,
1.));
#21785=DIRECTION('ref_axis',(9.07838619094529E-14,-1.,1.11716191852906E-13));
#21786=DIRECTION('',(9.74874922969709E-27,-1.11716191852906E-13,-1.));
#21787=DIRECTION('center_axis',(-1.00515054169548E-26,1.1518563880486E-13,
1.));
#21788=DIRECTION('ref_axis',(-8.72635297355373E-14,1.,-1.1518563880486E-13));
#21789=DIRECTION('center_axis',(-1.00515054169548E-26,1.1518563880486E-13,
1.));
#21790=DIRECTION('ref_axis',(-8.72635297355373E-14,1.,-1.1518563880486E-13));
#21791=DIRECTION('',(-1.00515054169548E-26,1.1518563880486E-13,1.));
#21792=DIRECTION('center_axis',(-1.00515054169548E-26,1.1518563880486E-13,
1.));
#21793=DIRECTION('ref_axis',(-8.72635297355373E-14,1.,-1.1518563880486E-13));
#21794=DIRECTION('',(1.00515054169548E-26,-1.1518563880486E-13,-1.));
#21795=DIRECTION('',(1.00515054169548E-26,-1.1518563880486E-13,-1.));
#21796=DIRECTION('center_axis',(-1.00515054169548E-26,1.1518563880486E-13,
1.));
#21797=DIRECTION('ref_axis',(-8.72635297355373E-14,1.,-1.1518563880486E-13));
#21798=DIRECTION('',(1.00515054169548E-26,-1.1518563880486E-13,-1.));
#21799=DIRECTION('center_axis',(0.868162779192246,0.382683432396709,0.315985410097158));
#21800=DIRECTION('ref_axis',(0.403349423721025,-0.915046032931632,1.06983183810373E-13));
#21801=DIRECTION('',(-0.328672675627568,-0.917633305084373,-0.223435426232604));
#21802=DIRECTION('center_axis',(0.868162779192246,0.382683432396709,0.315985410097158));
#21803=DIRECTION('ref_axis',(0.403349423721025,-0.915046032931632,1.06502267550115E-13));
#21804=DIRECTION('center_axis',(-1.00515054169548E-26,1.1518563880486E-13,
1.));
#21805=DIRECTION('ref_axis',(-8.72635297355372E-14,1.,-1.1518563880486E-13));
#21806=DIRECTION('center_axis',(-1.00515054169548E-26,1.1518563880486E-13,
1.));
#21807=DIRECTION('ref_axis',(-8.72635297355372E-14,1.,-1.1518563880486E-13));
#21808=DIRECTION('',(-1.00515054169548E-26,1.1518563880486E-13,1.));
#21809=DIRECTION('center_axis',(1.00515054169548E-26,-1.1518563880486E-13,
-1.));
#21810=DIRECTION('ref_axis',(-8.72635297355372E-14,1.,-1.1518563880486E-13));
#21811=DIRECTION('center_axis',(-1.00515054169548E-26,1.1518563880486E-13,
1.));
#21812=DIRECTION('ref_axis',(-8.67361737988404E-14,1.,-1.1518563880486E-13));
#21813=DIRECTION('center_axis',(-1.00515054169548E-26,1.1518563880486E-13,
1.));
#21814=DIRECTION('ref_axis',(-8.67361737988404E-14,1.,-1.1518563880486E-13));
#21815=DIRECTION('',(-1.00515054169548E-26,1.1518563880486E-13,1.));
#21816=DIRECTION('center_axis',(1.00515054169548E-26,-1.1518563880486E-13,
-1.));
#21817=DIRECTION('ref_axis',(-8.67361737988404E-14,1.,-1.1518563880486E-13));
#21818=DIRECTION('center_axis',(-1.00515054169548E-26,1.1518563880486E-13,
1.));
#21819=DIRECTION('ref_axis',(-8.72635297355372E-14,1.,-1.1518563880486E-13));
#21820=DIRECTION('center_axis',(-1.00515054169548E-26,1.1518563880486E-13,
1.));
#21821=DIRECTION('ref_axis',(-8.72635297355373E-14,1.,-1.1518563880486E-13));
#21822=DIRECTION('',(-1.00515054169548E-26,1.1518563880486E-13,1.));
#21823=DIRECTION('center_axis',(1.00515054169548E-26,-1.1518563880486E-13,
-1.));
#21824=DIRECTION('ref_axis',(-8.72635297355373E-14,1.,-1.1518563880486E-13));
#21825=DIRECTION('center_axis',(-1.00515054169548E-26,1.1518563880486E-13,
1.));
#21826=DIRECTION('ref_axis',(-8.67361737988404E-14,1.,-1.1518563880486E-13));
#21827=DIRECTION('center_axis',(-1.00515054169548E-26,1.1518563880486E-13,
1.));
#21828=DIRECTION('ref_axis',(-8.67361737988404E-14,1.,-1.1518563880486E-13));
#21829=DIRECTION('',(-1.00515054169548E-26,1.1518563880486E-13,1.));
#21830=DIRECTION('center_axis',(1.00515054169548E-26,-1.1518563880486E-13,
-1.));
#21831=DIRECTION('ref_axis',(-8.67361737988404E-14,1.,-1.1518563880486E-13));
#21832=DIRECTION('center_axis',(1.00515054169548E-26,-1.1518563880486E-13,
-1.));
#21833=DIRECTION('ref_axis',(8.72635297355373E-14,-1.,1.1518563880486E-13));
#21834=DIRECTION('center_axis',(1.00515054169548E-26,-1.1518563880486E-13,
-1.));
#21835=DIRECTION('ref_axis',(8.72635297355373E-14,-1.,1.1518563880486E-13));
#21836=DIRECTION('',(-1.00515054169548E-26,1.1518563880486E-13,1.));
#21837=DIRECTION('center_axis',(1.00515054169548E-26,-1.1518563880486E-13,
-1.));
#21838=DIRECTION('ref_axis',(8.72635297355373E-14,-1.,1.1518563880486E-13));
#21839=DIRECTION('',(-1.00515054169548E-26,1.1518563880486E-13,1.));
#21840=DIRECTION('center_axis',(-1.00515054169548E-26,1.1518563880486E-13,
1.));
#21841=DIRECTION('ref_axis',(8.72635297355373E-14,-1.,1.1518563880486E-13));
#21842=DIRECTION('',(-1.00515054169548E-26,1.1518563880486E-13,1.));
#21843=DIRECTION('center_axis',(1.00515054169548E-26,-1.1518563880486E-13,
-1.));
#21844=DIRECTION('ref_axis',(8.72635297355373E-14,-1.,1.1518563880486E-13));
#21845=DIRECTION('center_axis',(-1.00515054169548E-26,1.1518563880486E-13,
1.));
#21846=DIRECTION('ref_axis',(8.72635297355373E-14,-1.,1.1518563880486E-13));
#21847=DIRECTION('',(1.00515054169548E-26,-1.1518563880486E-13,-1.));
#21848=DIRECTION('center_axis',(1.00515054169548E-26,-1.1518563880486E-13,
-1.));
#21849=DIRECTION('ref_axis',(8.72635297355373E-14,-1.,1.1518563880486E-13));
#21850=DIRECTION('center_axis',(-8.72635297355373E-14,1.,-1.11716191852906E-13));
#21851=DIRECTION('ref_axis',(6.05512374515283E-29,-1.11716191852906E-13,
-1.));
#21852=DIRECTION('center_axis',(-8.72635297355373E-14,1.,-1.11716191852906E-13));
#21853=DIRECTION('ref_axis',(6.05512374515455E-29,-1.11716191852906E-13,
-1.));
#21854=DIRECTION('',(-8.72635297355373E-14,1.,-1.11716191852906E-13));
#21855=DIRECTION('center_axis',(8.72635297355373E-14,-1.,1.11716191852906E-13));
#21856=DIRECTION('ref_axis',(6.05512374515283E-29,-1.11716191852906E-13,
-1.));
#21857=DIRECTION('center_axis',(-8.72635297355373E-14,1.,-1.11716191852906E-13));
#21858=DIRECTION('ref_axis',(6.05512374515455E-29,-1.11716191852906E-13,
-1.));
#21859=DIRECTION('center_axis',(-8.72635297355373E-14,1.,-1.11716191852906E-13));
#21860=DIRECTION('ref_axis',(6.05512374515455E-29,-1.11716191852906E-13,
-1.));
#21861=DIRECTION('',(-8.72635297355373E-14,1.,-1.11716191852906E-13));
#21862=DIRECTION('center_axis',(-8.72635297355373E-14,1.,-1.11716191852906E-13));
#21863=DIRECTION('ref_axis',(6.05512374515455E-29,-1.11716191852906E-13,
-1.));
#21864=DIRECTION('center_axis',(1.00515054169548E-26,-1.1518563880486E-13,
-1.));
#21865=DIRECTION('ref_axis',(8.72635297355373E-14,-1.,1.1518563880486E-13));
#21866=DIRECTION('',(6.16180380206417E-14,-0.707106781186466,0.707106781186629));
#21867=DIRECTION('center_axis',(1.00515054169548E-26,-1.1518563880486E-13,
-1.));
#21868=DIRECTION('ref_axis',(8.72635297355373E-14,-1.,1.1518563880486E-13));
#21869=DIRECTION('center_axis',(8.72635297355373E-14,-1.,1.1518563880486E-13));
#21870=DIRECTION('ref_axis',(-1.73003535575891E-29,1.1518563880486E-13,
1.));
#21871=DIRECTION('center_axis',(8.72635297355373E-14,-1.,1.1518563880486E-13));
#21872=DIRECTION('ref_axis',(-1.73003535575891E-29,1.1518563880486E-13,
1.));
#21873=DIRECTION('',(-8.72635297355373E-14,1.,-1.1518563880486E-13));
#21874=DIRECTION('center_axis',(8.72635297355373E-14,-1.,1.1518563880486E-13));
#21875=DIRECTION('ref_axis',(-1.73003535575891E-29,1.1518563880486E-13,
1.));
#21876=DIRECTION('center_axis',(8.72635297355373E-14,-1.,1.1518563880486E-13));
#21877=DIRECTION('ref_axis',(-1.73003535575891E-29,1.1518563880486E-13,
1.));
#21878=DIRECTION('center_axis',(8.72635297355373E-14,-1.,1.1518563880486E-13));
#21879=DIRECTION('ref_axis',(-1.73003535575891E-29,1.1518563880486E-13,
1.));
#21880=DIRECTION('',(-8.72635297355373E-14,1.,-1.1518563880486E-13));
#21881=DIRECTION('center_axis',(8.72635297355373E-14,-1.,1.1518563880486E-13));
#21882=DIRECTION('ref_axis',(-1.73003535575891E-29,1.1518563880486E-13,
1.));
#21883=DIRECTION('center_axis',(-1.00515054169548E-26,1.1518563880486E-13,
1.));
#21884=DIRECTION('ref_axis',(-8.78926561161581E-14,1.,-1.1518563880486E-13));
#21885=DIRECTION('center_axis',(-1.00515054169548E-26,1.1518563880486E-13,
1.));
#21886=DIRECTION('ref_axis',(-8.78926561161581E-14,1.,-1.1518563880486E-13));
#21887=DIRECTION('',(1.00515054169548E-26,-1.1518563880486E-13,-1.));
#21888=DIRECTION('center_axis',(-1.00515054169548E-26,1.1518563880486E-13,
1.));
#21889=DIRECTION('ref_axis',(-8.78926561161581E-14,1.,-1.1518563880486E-13));
#21890=DIRECTION('center_axis',(-1.00515054169548E-26,1.1518563880486E-13,
1.));
#21891=DIRECTION('ref_axis',(-8.78926561160683E-14,1.,-1.1518563880486E-13));
#21892=DIRECTION('center_axis',(-1.00515054169548E-26,1.1518563880486E-13,
1.));
#21893=DIRECTION('ref_axis',(-8.78926561160683E-14,1.,-1.1518563880486E-13));
#21894=DIRECTION('',(1.00515054169548E-26,-1.1518563880486E-13,-1.));
#21895=DIRECTION('center_axis',(-1.00515054169548E-26,1.1518563880486E-13,
1.));
#21896=DIRECTION('ref_axis',(-8.78926561160683E-14,1.,-1.1518563880486E-13));
#21897=DIRECTION('center_axis',(-1.00515054169548E-26,1.1518563880486E-13,
1.));
#21898=DIRECTION('ref_axis',(-8.78926561160967E-14,1.,-1.1518563880486E-13));
#21899=DIRECTION('center_axis',(-1.00515054169548E-26,1.1518563880486E-13,
1.));
#21900=DIRECTION('ref_axis',(-8.78926561160967E-14,1.,-1.1518563880486E-13));
#21901=DIRECTION('',(1.00515054169548E-26,-1.1518563880486E-13,-1.));
#21902=DIRECTION('center_axis',(-1.00515054169548E-26,1.1518563880486E-13,
1.));
#21903=DIRECTION('ref_axis',(-8.78926561160967E-14,1.,-1.1518563880486E-13));
#21904=DIRECTION('center_axis',(-1.00515054169548E-26,1.1518563880486E-13,
1.));
#21905=DIRECTION('ref_axis',(-8.78926561161797E-14,1.,-1.1518563880486E-13));
#21906=DIRECTION('center_axis',(-1.00515054169548E-26,1.1518563880486E-13,
1.));
#21907=DIRECTION('ref_axis',(-8.78926561161797E-14,1.,-1.1518563880486E-13));
#21908=DIRECTION('',(1.00515054169548E-26,-1.1518563880486E-13,-1.));
#21909=DIRECTION('center_axis',(-1.00515054169548E-26,1.1518563880486E-13,
1.));
#21910=DIRECTION('ref_axis',(-8.78926561161797E-14,1.,-1.1518563880486E-13));
#21911=DIRECTION('center_axis',(1.00515054169548E-26,-1.1518563880486E-13,
-1.));
#21912=DIRECTION('ref_axis',(8.72635297355373E-14,-1.,1.1518563880486E-13));
#21913=DIRECTION('center_axis',(1.00515054169548E-26,-1.1518563880486E-13,
-1.));
#21914=DIRECTION('ref_axis',(8.72635297355373E-14,-1.,1.1518563880486E-13));
#21915=DIRECTION('',(-1.00515054169548E-26,1.1518563880486E-13,1.));
#21916=DIRECTION('center_axis',(-1.00515054169548E-26,1.1518563880486E-13,
1.));
#21917=DIRECTION('ref_axis',(8.72635297355373E-14,-1.,1.1518563880486E-13));
#21918=DIRECTION('',(1.00515054169548E-26,-1.1518563880486E-13,-1.));
#21919=DIRECTION('center_axis',(1.00515054169548E-26,-1.1518563880486E-13,
-1.));
#21920=DIRECTION('ref_axis',(8.72635297355373E-14,-1.,1.1518563880486E-13));
#21921=DIRECTION('',(1.00515054169548E-26,-1.1518563880486E-13,-1.));
#21922=DIRECTION('center_axis',(-1.00515054169548E-26,1.1518563880486E-13,
1.));
#21923=DIRECTION('ref_axis',(8.72635297355373E-14,-1.,1.1518563880486E-13));
#21924=DIRECTION('center_axis',(-1.00515054169548E-26,1.1518563880486E-13,
1.));
#21925=DIRECTION('ref_axis',(8.72635297355373E-14,-1.,1.1518563880486E-13));
#21926=DIRECTION('center_axis',(1.05148106564929E-14,1.13041557302278E-13,
1.));
#21927=DIRECTION('ref_axis',(1.,8.72630157433963E-14,-1.05148106565028E-14));
#21928=DIRECTION('center_axis',(1.05148106564929E-14,1.13041557302278E-13,
1.));
#21929=DIRECTION('ref_axis',(1.,8.72632848014737E-14,-1.05148106565028E-14));
#21930=DIRECTION('',(-0.0174340297464476,-0.000800685489193615,-0.999847695156391));
#21931=DIRECTION('center_axis',(1.05148106564929E-14,1.13041557302278E-13,
1.));
#21932=DIRECTION('ref_axis',(1.,8.72630157433963E-14,-1.05148106565028E-14));
#21933=DIRECTION('',(-0.0174340297464478,0.000800685488960295,-0.999847695156391));
#21934=DIRECTION('center_axis',(5.13992141019283E-16,1.1518563880486E-13,
1.));
#21935=DIRECTION('ref_axis',(1.,8.72635297355373E-14,-5.13992141029335E-16));
#21936=DIRECTION('center_axis',(-1.00515054169548E-26,1.1518563880486E-13,
1.));
#21937=DIRECTION('ref_axis',(8.72635297355373E-14,-1.,1.1518563880486E-13));
#21938=DIRECTION('center_axis',(-1.00515054169548E-26,1.1518563880486E-13,
1.));
#21939=DIRECTION('ref_axis',(8.72635297355373E-14,-1.,1.1518563880486E-13));
#21940=DIRECTION('',(-0.707106781186547,1.96573170623249E-14,0.707106781186548));
#21941=DIRECTION('center_axis',(-1.00515054169548E-26,1.1518563880486E-13,
1.));
#21942=DIRECTION('ref_axis',(-8.72635297355373E-14,1.,-1.1518563880486E-13));
#21943=DIRECTION('center_axis',(-1.00515054169548E-26,1.1518563880486E-13,
1.));
#21944=DIRECTION('ref_axis',(-8.72635297355373E-14,1.,-1.1518563880486E-13));
#21945=DIRECTION('center_axis',(-1.00515054169548E-26,1.1518563880486E-13,
1.));
#21946=DIRECTION('ref_axis',(-8.72635297355373E-14,1.,-1.1518563880486E-13));
#21947=DIRECTION('',(-1.00515054169548E-26,1.1518563880486E-13,1.));
#21948=DIRECTION('center_axis',(1.04893682793573E-14,1.13034729017238E-13,
1.));
#21949=DIRECTION('ref_axis',(1.,8.72628520516316E-14,-1.04893682793672E-14));
#21950=DIRECTION('center_axis',(1.50814224405608E-9,1.30680347155798E-11,
1.));
#21951=DIRECTION('ref_axis',(0.999950224327263,0.0099774178952433,-1.50819757644053E-9));
#21952=DIRECTION('center_axis',(2.2737638208062E-9,5.96781185745539E-11,
1.));
#21953=DIRECTION('ref_axis',(0.999629828344744,0.0272067323186488,-2.27454576389334E-9));
#21954=DIRECTION('',(-0.0174340340546636,-0.000800591677107547,-0.999847695156391));
#21955=DIRECTION('center_axis',(1.04893682793573E-14,1.13034729017238E-13,
1.));
#21956=DIRECTION('ref_axis',(1.,8.72628520516316E-14,-1.04893682793672E-14));
#21957=DIRECTION('',(-0.0174340340546638,0.00080059167687424,-0.999847695156391));
#21958=DIRECTION('center_axis',(2.01391717416503E-9,-5.2395782353962E-11,
1.));
#21959=DIRECTION('ref_axis',(0.999686135569083,-0.0250525517852406,-2.01459769357307E-9));
#21960=DIRECTION('center_axis',(1.34057310888677E-9,-1.13635839552688E-11,
1.));
#21961=DIRECTION('ref_axis',(0.999970713945725,-0.00765318566846746,-1.34062078067377E-9));
#21962=DIRECTION('center_axis',(1.,8.72635297355373E-14,0.));
#21963=DIRECTION('ref_axis',(8.72635297355373E-14,-1.,1.13545536609336E-13));
#21964=DIRECTION('center_axis',(-1.,-8.55363631858458E-14,2.53597807885338E-16));
#21965=DIRECTION('ref_axis',(8.57899609937212E-14,-1.,1.21115239049959E-13));
#21966=DIRECTION('',(-1.,-8.72635297355373E-14,0.));
#21967=DIRECTION('center_axis',(-1.,-8.72635297355373E-14,0.));
#21968=DIRECTION('ref_axis',(8.72635297355373E-14,-1.,1.19853621976522E-13));
#21969=DIRECTION('center_axis',(1.,8.72635297355373E-14,0.));
#21970=DIRECTION('ref_axis',(8.72635297355373E-14,-1.,1.13545536609336E-13));
#21971=DIRECTION('center_axis',(-1.,-8.55363631858455E-14,2.53597807885001E-16));
#21972=DIRECTION('ref_axis',(8.57899609937217E-14,-1.,1.2111523904996E-13));
#21973=DIRECTION('',(-1.,-8.72635297355373E-14,0.));
#21974=DIRECTION('center_axis',(-1.,-8.72635297355373E-14,0.));
#21975=DIRECTION('ref_axis',(8.72635297355373E-14,-1.,1.19853621976522E-13));
#21976=DIRECTION('center_axis',(1.00515054169548E-26,-1.1518563880486E-13,
-1.));
#21977=DIRECTION('ref_axis',(8.72635297355373E-14,-1.,1.1518563880486E-13));
#21978=DIRECTION('',(-6.16180380185814E-14,0.707106781162823,-0.707106781210272));
#21979=DIRECTION('center_axis',(-1.00515054169548E-26,1.1518563880486E-13,
1.));
#21980=DIRECTION('ref_axis',(8.72635297355373E-14,-1.,1.1518563880486E-13));
#21981=DIRECTION('center_axis',(1.00515054169548E-26,-1.1518563880486E-13,
-1.));
#21982=DIRECTION('ref_axis',(8.72635297355373E-14,-1.,1.1518563880486E-13));
#21983=DIRECTION('center_axis',(-8.07434927010188E-16,1.13848324707016E-13,
1.));
#21984=DIRECTION('ref_axis',(-8.57535022254239E-14,1.,-1.14655759634016E-13));
#21985=DIRECTION('',(1.00515054169548E-26,-1.1518563880486E-13,-1.));
#21986=DIRECTION('center_axis',(-1.00515054169548E-26,1.1518563880486E-13,
1.));
#21987=DIRECTION('ref_axis',(8.72635297355373E-14,-1.,1.1518563880486E-13));
#21988=DIRECTION('center_axis',(-1.00515054169548E-26,1.1518563880486E-13,
1.));
#21989=DIRECTION('ref_axis',(8.72635297355373E-14,-1.,1.1518563880486E-13));
#21990=DIRECTION('center_axis',(-1.04744440165193E-14,-1.15185638804861E-13,
-1.));
#21991=DIRECTION('ref_axis',(-1.,-8.72677046689168E-14,1.04744440165294E-14));
#21992=DIRECTION('center_axis',(-1.60317441773188E-14,-1.30010586908455E-13,
-1.));
#21993=DIRECTION('ref_axis',(-0.986663993658372,0.162770278669396,-5.1459919581511E-15));
#21994=DIRECTION('',(-1.04744440165193E-14,-1.15185638804861E-13,-1.));
#21995=DIRECTION('center_axis',(-5.8420956475864E-12,5.24858042098029E-13,
1.));
#21996=DIRECTION('ref_axis',(-1.,-8.33007448225695E-14,-5.84228425464237E-12));
#21997=DIRECTION('',(-1.04744440165193E-14,-1.15185638804861E-13,-1.));
#21998=DIRECTION('center_axis',(-1.00515054169548E-26,1.1518563880486E-13,
1.));
#21999=DIRECTION('ref_axis',(-8.72635297355373E-14,1.,-1.1518563880486E-13));
#22000=DIRECTION('',(7.81604095158039E-14,-0.894427190977678,0.447213595544433));
#22001=DIRECTION('center_axis',(7.90669341981024E-5,-6.79899070760606E-6,
-0.999999996851097));
#22002=DIRECTION('ref_axis',(-0.224409606993171,0.974494909014575,-2.4368961537286E-5));
#22003=DIRECTION('center_axis',(4.84900603469004E-5,2.12716297860176E-5,
-0.999999998598116));
#22004=DIRECTION('ref_axis',(-0.215549302917957,0.97649295845136,1.03195980090732E-5));
#22005=DIRECTION('',(-0.476471251976903,-0.412057254805414,-0.776649190305242));
#22006=DIRECTION('',(0.497089462473265,0.150347978283572,0.854574485767088));
#22007=DIRECTION('',(0.49708946264798,-0.150347978462221,0.85457448563403));
#22008=DIRECTION('',(0.472361792915602,-0.100907068159122,0.875609559215229));
#22009=DIRECTION('center_axis',(4.84900605051656E-5,-2.12716300746791E-5,
-0.999999998598116));
#22010=DIRECTION('ref_axis',(0.215549302836865,0.97649295846926,-1.03195982611481E-5));
#22011=DIRECTION('',(-0.47647125197697,0.412057254805155,-0.776649190305339));
#22012=DIRECTION('',(-0.379976420578336,0.59082305053514,-0.711720480779376));
#22013=DIRECTION('center_axis',(1.42705873244029E-5,-3.83465092369397E-5,
-0.999999999162948));
#22014=DIRECTION('ref_axis',(0.857448829753204,0.514569241500769,-7.49563577732842E-6));
#22015=DIRECTION('',(-0.590708354574789,0.380106497268313,-0.711746226242163));
#22016=DIRECTION('',(-0.411902009107452,0.476603463260479,-0.776650419237228));
#22017=DIRECTION('center_axis',(-1.2742627722323E-5,-2.90510924139551E-5,
-0.99999999949683));
#22018=DIRECTION('ref_axis',(0.976471046734733,-0.215648544744935,-6.17798123095627E-6));
#22019=DIRECTION('center_axis',(-2.2112189231786E-5,-7.9504155517196E-6,
-0.999999999723921));
#22020=DIRECTION('ref_axis',(-0.574484253249288,0.818515633772637,6.19556509616842E-6));
#22021=DIRECTION('center_axis',(-8.72635297355373E-14,1.,-1.1518563880486E-13));
#22022=DIRECTION('ref_axis',(1.00515054169548E-26,-1.1518563880486E-13,
-1.));
#22023=DIRECTION('',(-0.866025403789923,-1.79796141740169E-14,0.4999999999905));
#22024=DIRECTION('',(-1.00515054169548E-26,1.1518563880486E-13,1.));
#22025=DIRECTION('',(0.866025403789923,1.33165252976688E-13,0.4999999999905));
#22026=DIRECTION('',(0.866025403789923,1.79796141740169E-14,-0.4999999999905));
#22027=DIRECTION('',(1.00515054169548E-26,-1.1518563880486E-13,-1.));
#22028=DIRECTION('',(-0.866025403789923,-1.33165252976688E-13,-0.4999999999905));
#22029=DIRECTION('center_axis',(-8.72635297355373E-14,1.,-1.1518563880486E-13));
#22030=DIRECTION('ref_axis',(1.00515054169548E-26,-1.1518563880486E-13,
-1.));
#22031=DIRECTION('',(-0.866025403789923,-1.79796141740169E-14,0.4999999999905));
#22032=DIRECTION('',(-1.00515054169548E-26,1.1518563880486E-13,1.));
#22033=DIRECTION('',(0.866025403789923,1.33165252976688E-13,0.4999999999905));
#22034=DIRECTION('',(0.866025403789923,1.79796141740169E-14,-0.4999999999905));
#22035=DIRECTION('',(1.00515054169548E-26,-1.1518563880486E-13,-1.));
#22036=DIRECTION('',(-0.866025403789923,-1.33165252976688E-13,-0.4999999999905));
#22037=DIRECTION('center_axis',(-8.72635297355373E-14,1.,-1.1518563880486E-13));
#22038=DIRECTION('ref_axis',(1.00515054169548E-26,-1.1518563880486E-13,
-1.));
#22039=DIRECTION('',(-0.866025403789923,-1.79796141740169E-14,0.4999999999905));
#22040=DIRECTION('',(-1.00515054169548E-26,1.1518563880486E-13,1.));
#22041=DIRECTION('',(0.866025403789923,1.33165252976688E-13,0.4999999999905));
#22042=DIRECTION('',(0.866025403789923,1.79796141740169E-14,-0.4999999999905));
#22043=DIRECTION('',(1.00515054169548E-26,-1.1518563880486E-13,-1.));
#22044=DIRECTION('',(-0.866025403789923,-1.33165252976688E-13,-0.4999999999905));
#22045=DIRECTION('center_axis',(-8.72635297355373E-14,1.,-1.1518563880486E-13));
#22046=DIRECTION('ref_axis',(1.00515054169548E-26,-1.1518563880486E-13,
-1.));
#22047=DIRECTION('',(-0.866025403789923,-1.79796141740169E-14,0.4999999999905));
#22048=DIRECTION('',(-1.00515054169548E-26,1.1518563880486E-13,1.));
#22049=DIRECTION('',(0.866025403789923,1.33165252976688E-13,0.4999999999905));
#22050=DIRECTION('',(0.866025403789923,1.79796141740169E-14,-0.4999999999905));
#22051=DIRECTION('',(1.00515054169548E-26,-1.1518563880486E-13,-1.));
#22052=DIRECTION('',(-0.866025403789923,-1.33165252976688E-13,-0.4999999999905));
#22053=DIRECTION('center_axis',(-1.04744440165193E-14,-1.15185638804861E-13,
-1.));
#22054=DIRECTION('ref_axis',(-1.,-8.72635297355361E-14,1.04744440165294E-14));
#22055=DIRECTION('center_axis',(1.27156302261967E-12,-7.67259042032779E-13,
-1.));
#22056=DIRECTION('ref_axis',(0.707106781186604,-0.707106781186491,1.44328993201271E-12));
#22057=DIRECTION('',(-0.707106781186489,-0.707106781186606,8.14485462942204E-14));
#22058=DIRECTION('center_axis',(-5.76880098885803E-15,-2.11163646621927E-13,
-1.));
#22059=DIRECTION('ref_axis',(0.162770278669586,-0.98666399365834,2.08721928629528E-13));
#22060=DIRECTION('center_axis',(2.90371050762764E-14,-3.54407276356552E-13,
-1.));
#22061=DIRECTION('ref_axis',(9.61069664125861E-14,-1.,3.54281754041935E-13));
#22062=DIRECTION('center_axis',(-3.74976319533066E-13,-9.52526981242744E-13,
-1.));
#22063=DIRECTION('ref_axis',(-0.70710678118649,-0.707106781186605,9.37028232783635E-13));
#22064=DIRECTION('',(-0.707106781186605,0.70710678118649,-8.14485462942213E-14));
#22065=DIRECTION('center_axis',(1.28789942775155E-13,-4.80738143802119E-14,
-1.));
#22066=DIRECTION('ref_axis',(-0.986663993658341,-0.162770278669579,-1.19904086659517E-13));
#22067=DIRECTION('center_axis',(-1.28789942775156E-13,-4.80738143802258E-14,
-1.));
#22068=DIRECTION('ref_axis',(-0.707106781186605,0.70710678118649,5.77315972805082E-14));
#22069=DIRECTION('',(0.70710678118649,0.707106781186605,-8.14485462942203E-14));
#22070=DIRECTION('center_axis',(-1.89685730694799E-13,1.62833466326211E-13,
-1.));
#22071=DIRECTION('ref_axis',(-0.162770278669582,0.986663993658341,1.90958360235528E-13));
#22072=DIRECTION('center_axis',(-1.08828435367454E-13,8.83049349377018E-13,
-1.));
#22073=DIRECTION('ref_axis',(-9.16685483161296E-14,1.,8.83131389125757E-13));
#22074=DIRECTION('center_axis',(-4.23050133913277E-14,-8.23737038467554E-14,
-1.));
#22075=DIRECTION('ref_axis',(0.707106781186495,0.7071067811866,-8.88178419700125E-14));
#22076=DIRECTION('',(0.707106781186606,-0.707106781186489,8.14485462942212E-14));
#22077=DIRECTION('center_axis',(1.73292240336301E-13,-3.33769382396367E-14,
-1.));
#22078=DIRECTION('ref_axis',(0.986663993658341,0.162770278669582,1.64313007644524E-13));
#22079=DIRECTION('center_axis',(2.07777251728183E-13,-1.02140959738333E-13,
-1.));
#22080=DIRECTION('ref_axis',(0.986663993658371,-0.1627702786694,2.21673499735742E-13));
#22081=DIRECTION('center_axis',(1.,8.72635297355373E-14,0.));
#22082=DIRECTION('ref_axis',(8.72635297355373E-14,-1.,1.1518563880486E-13));
#22083=DIRECTION('',(4.36317648683653E-14,-0.500000000006838,-0.866025403780491));
#22084=DIRECTION('',(-4.36317648683479E-14,0.500000000006639,-0.866025403780606));
#22085=DIRECTION('',(-8.72635297355373E-14,1.,-1.1518563880486E-13));
#22086=DIRECTION('',(-4.36317648683653E-14,0.500000000006838,0.866025403780491));
#22087=DIRECTION('',(4.36317648683479E-14,-0.500000000006639,0.866025403780606));
#22088=DIRECTION('',(8.72635297355373E-14,-1.,1.1518563880486E-13));
#22089=DIRECTION('center_axis',(1.,8.72635297355373E-14,0.));
#22090=DIRECTION('ref_axis',(8.72635297355373E-14,-1.,1.1518563880486E-13));
#22091=DIRECTION('',(4.36317648683653E-14,-0.500000000006838,-0.866025403780491));
#22092=DIRECTION('',(-4.36317648683479E-14,0.500000000006639,-0.866025403780606));
#22093=DIRECTION('',(-8.72635297355373E-14,1.,-1.1518563880486E-13));
#22094=DIRECTION('',(-4.36317648683653E-14,0.500000000006838,0.866025403780491));
#22095=DIRECTION('',(4.36317648683479E-14,-0.500000000006639,0.866025403780606));
#22096=DIRECTION('',(8.72635297355373E-14,-1.,1.1518563880486E-13));
#22097=DIRECTION('center_axis',(-0.4999999999905,-1.43385454223719E-13,
-0.866025403789923));
#22098=DIRECTION('ref_axis',(-0.866025403789923,-1.79796141740169E-14,0.4999999999905));
#22099=DIRECTION('',(-0.866025403789921,-1.79796141740162E-14,0.499999999990505));
#22100=DIRECTION('',(8.72635297355373E-14,-1.,1.1518563880486E-13));
#22101=DIRECTION('',(-8.72635297355373E-14,1.,-1.1518563880486E-13));
#22102=DIRECTION('center_axis',(-1.,-8.72635297355373E-14,0.));
#22103=DIRECTION('ref_axis',(-8.72635297355373E-14,1.,-1.1518563880486E-13));
#22104=DIRECTION('',(-1.00515054169548E-26,1.1518563880486E-13,1.));
#22105=DIRECTION('',(8.72635297355373E-14,-1.,1.1518563880486E-13));
#22106=DIRECTION('center_axis',(-0.4999999999905,5.61219244898395E-14,0.866025403789923));
#22107=DIRECTION('ref_axis',(0.866025403789923,1.33165252976688E-13,0.4999999999905));
#22108=DIRECTION('',(0.866025403789921,1.33165252976689E-13,0.499999999990505));
#22109=DIRECTION('',(8.72635297355373E-14,-1.,1.1518563880486E-13));
#22110=DIRECTION('center_axis',(0.4999999999905,1.43385454223719E-13,0.866025403789923));
#22111=DIRECTION('ref_axis',(0.866025403789923,1.79796141740169E-14,-0.4999999999905));
#22112=DIRECTION('',(0.866025403789921,1.79796141740163E-14,-0.499999999990504));
#22113=DIRECTION('',(8.72635297355373E-14,-1.,1.1518563880486E-13));
#22114=DIRECTION('center_axis',(1.,8.72635297355373E-14,0.));
#22115=DIRECTION('ref_axis',(8.72635297355373E-14,-1.,1.1518563880486E-13));
#22116=DIRECTION('',(1.00515054169548E-26,-1.1518563880486E-13,-1.));
#22117=DIRECTION('',(8.72635297355373E-14,-1.,1.1518563880486E-13));
#22118=DIRECTION('center_axis',(0.4999999999905,-5.61219244898395E-14,-0.866025403789923));
#22119=DIRECTION('ref_axis',(-0.866025403789923,-1.33165252976688E-13,-0.4999999999905));
#22120=DIRECTION('',(-0.866025403789921,-1.33165252976689E-13,-0.499999999990504));
#22121=DIRECTION('center_axis',(-1.00515054169548E-26,1.1518563880486E-13,
1.));
#22122=DIRECTION('ref_axis',(-8.72635297355373E-14,1.,-1.1518563880486E-13));
#22123=DIRECTION('',(-8.72635297355373E-14,1.,-1.1518563880486E-13));
#22124=DIRECTION('',(-1.,-8.72635297355373E-14,0.));
#22125=DIRECTION('',(-8.72635297355373E-14,1.,-1.1518563880486E-13));
#22126=DIRECTION('',(-1.,-8.72635297355373E-14,0.));
#22127=DIRECTION('center_axis',(4.90114831233627E-14,4.90114831233761E-14,
1.));
#22128=DIRECTION('ref_axis',(-8.50113630284402E-14,1.,-5.07530525542927E-14));
#22129=DIRECTION('center_axis',(8.72635297355373E-14,-1.,1.1518563880486E-13));
#22130=DIRECTION('ref_axis',(-1.73003535575891E-29,1.1518563880486E-13,
1.));
#22131=DIRECTION('',(-8.72635297355373E-14,1.,-1.1518563880486E-13));
#22132=DIRECTION('center_axis',(5.42890133665177E-14,-1.,1.46185544222939E-13));
#22133=DIRECTION('ref_axis',(-1.,-5.32907051820067E-14,1.01506105108584E-14));
#22134=DIRECTION('center_axis',(8.05891463095976E-14,-1.,1.17347758652129E-13));
#22135=DIRECTION('ref_axis',(-1.,-8.12048840868677E-14,-1.21807326130302E-13));
#22136=DIRECTION('center_axis',(-1.,-8.72635297355373E-14,0.));
#22137=DIRECTION('ref_axis',(-8.72635297355373E-14,1.,-1.1518563880486E-13));
#22138=DIRECTION('',(1.00515054169548E-26,-1.1518563880486E-13,-1.));
#22139=DIRECTION('',(1.00515054169548E-26,-1.1518563880486E-13,-1.));
#22140=DIRECTION('',(8.72635297355373E-14,-1.,1.1518563880486E-13));
#22141=DIRECTION('center_axis',(-1.,-8.81911644086169E-14,6.42148752471851E-16));
#22142=DIRECTION('ref_axis',(-6.34413156928658E-16,-1.14194368247158E-13,
-1.));
#22143=DIRECTION('center_axis',(0.4999999999905,-5.61219244898395E-14,-0.866025403789923));
#22144=DIRECTION('ref_axis',(-0.866025403789923,-1.33165252976688E-13,-0.4999999999905));
#22145=DIRECTION('',(0.866025403789921,1.33165252976689E-13,0.499999999990504));
#22146=DIRECTION('',(8.72635297355373E-14,-1.,1.1518563880486E-13));
#22147=DIRECTION('',(-8.72635297355373E-14,1.,-1.1518563880486E-13));
#22148=DIRECTION('center_axis',(1.,8.72635297355373E-14,0.));
#22149=DIRECTION('ref_axis',(8.72635297355373E-14,-1.,1.1518563880486E-13));
#22150=DIRECTION('',(-1.00515054169548E-26,1.1518563880486E-13,1.));
#22151=DIRECTION('',(-8.72635297355373E-14,1.,-1.1518563880486E-13));
#22152=DIRECTION('center_axis',(0.4999999999905,1.43385454223719E-13,0.866025403789923));
#22153=DIRECTION('ref_axis',(0.866025403789923,1.79796141740169E-14,-0.4999999999905));
#22154=DIRECTION('',(-0.866025403789921,-1.79796141740163E-14,0.499999999990504));
#22155=DIRECTION('',(-8.72635297355373E-14,1.,-1.1518563880486E-13));
#22156=DIRECTION('center_axis',(-0.4999999999905,5.61219244898395E-14,0.866025403789923));
#22157=DIRECTION('ref_axis',(0.866025403789923,1.33165252976688E-13,0.4999999999905));
#22158=DIRECTION('',(-0.866025403789921,-1.33165252976689E-13,-0.499999999990505));
#22159=DIRECTION('',(-8.72635297355373E-14,1.,-1.1518563880486E-13));
#22160=DIRECTION('center_axis',(-1.,-8.72635297355373E-14,0.));
#22161=DIRECTION('ref_axis',(-8.72635297355373E-14,1.,-1.1518563880486E-13));
#22162=DIRECTION('',(1.00515054169548E-26,-1.1518563880486E-13,-1.));
#22163=DIRECTION('',(-8.72635297355373E-14,1.,-1.1518563880486E-13));
#22164=DIRECTION('center_axis',(-0.4999999999905,-1.43385454223719E-13,
-0.866025403789923));
#22165=DIRECTION('ref_axis',(-0.866025403789923,-1.79796141740169E-14,0.4999999999905));
#22166=DIRECTION('',(0.866025403789921,1.79796141740162E-14,-0.499999999990505));
#22167=DIRECTION('center_axis',(-1.00515054169548E-26,1.1518563880486E-13,
1.));
#22168=DIRECTION('ref_axis',(-8.72635297355373E-14,1.,-1.1518563880486E-13));
#22169=DIRECTION('',(-1.,-8.72635297355373E-14,0.));
#22170=DIRECTION('',(8.72635297355373E-14,-1.,1.1518563880486E-13));
#22171=DIRECTION('',(1.,8.72635297355373E-14,0.));
#22172=DIRECTION('',(8.72635297355373E-14,-1.,1.1518563880486E-13));
#22173=DIRECTION('center_axis',(-4.90114831233668E-14,4.90114831233573E-14,
1.));
#22174=DIRECTION('ref_axis',(-1.,-1.06581410364015E-13,-5.07530525542928E-14));
#22175=DIRECTION('center_axis',(-8.72635297355373E-14,1.,-1.1518563880486E-13));
#22176=DIRECTION('ref_axis',(1.73003535575891E-29,-1.1518563880486E-13,
-1.));
#22177=DIRECTION('',(8.72635297355373E-14,-1.,1.1518563880486E-13));
#22178=DIRECTION('center_axis',(-5.82913089187531E-14,1.,-8.87431404513285E-14));
#22179=DIRECTION('ref_axis',(1.,5.83660104374363E-14,1.01506105108585E-14));
#22180=DIRECTION('center_axis',(7.05441796996118E-14,-1.,1.009960112322E-13));
#22181=DIRECTION('ref_axis',(1.26882631385732E-15,1.01506105108585E-13,
1.));
#22182=DIRECTION('center_axis',(1.,8.72635297355373E-14,0.));
#22183=DIRECTION('ref_axis',(8.72635297355373E-14,-1.,1.1518563880486E-13));
#22184=DIRECTION('',(-8.72635297355373E-14,1.,-1.1518563880486E-13));
#22185=DIRECTION('',(1.00515054169548E-26,-1.1518563880486E-13,-1.));
#22186=DIRECTION('',(-1.00515054169548E-26,1.1518563880486E-13,1.));
#22187=DIRECTION('center_axis',(1.,8.90883600992922E-14,-2.80817075700569E-15));
#22188=DIRECTION('ref_axis',(-8.88178419700117E-14,1.,-1.01506105108585E-14));
#22189=DIRECTION('center_axis',(0.4999999999905,-5.61219244898395E-14,-0.866025403789923));
#22190=DIRECTION('ref_axis',(-0.866025403789923,-1.33165252976688E-13,-0.4999999999905));
#22191=DIRECTION('',(0.866025403789926,1.33165252976688E-13,0.499999999990495));
#22192=DIRECTION('',(8.72635297355373E-14,-1.,1.1518563880486E-13));
#22193=DIRECTION('',(-8.72635297355373E-14,1.,-1.1518563880486E-13));
#22194=DIRECTION('center_axis',(1.,8.72635297355373E-14,0.));
#22195=DIRECTION('ref_axis',(8.72635297355373E-14,-1.,1.1518563880486E-13));
#22196=DIRECTION('',(-1.00515054169548E-26,1.1518563880486E-13,1.));
#22197=DIRECTION('',(-8.72635297355373E-14,1.,-1.1518563880486E-13));
#22198=DIRECTION('center_axis',(0.4999999999905,1.43385454223719E-13,0.866025403789923));
#22199=DIRECTION('ref_axis',(0.866025403789923,1.79796141740169E-14,-0.4999999999905));
#22200=DIRECTION('',(-0.866025403789926,-1.79796141740178E-14,0.499999999990495));
#22201=DIRECTION('',(-8.72635297355373E-14,1.,-1.1518563880486E-13));
#22202=DIRECTION('center_axis',(-0.4999999999905,5.61219244898395E-14,0.866025403789923));
#22203=DIRECTION('ref_axis',(0.866025403789923,1.33165252976688E-13,0.4999999999905));
#22204=DIRECTION('',(-0.866025403789926,-1.33165252976688E-13,-0.499999999990495));
#22205=DIRECTION('',(-8.72635297355373E-14,1.,-1.1518563880486E-13));
#22206=DIRECTION('center_axis',(-1.,-8.72635297355373E-14,0.));
#22207=DIRECTION('ref_axis',(-8.72635297355373E-14,1.,-1.1518563880486E-13));
#22208=DIRECTION('',(1.00515054169548E-26,-1.1518563880486E-13,-1.));
#22209=DIRECTION('',(-8.72635297355373E-14,1.,-1.1518563880486E-13));
#22210=DIRECTION('center_axis',(-0.4999999999905,-1.43385454223719E-13,
-0.866025403789923));
#22211=DIRECTION('ref_axis',(-0.866025403789923,-1.79796141740169E-14,0.4999999999905));
#22212=DIRECTION('',(0.866025403789926,1.79796141740177E-14,-0.499999999990495));
#22213=DIRECTION('center_axis',(1.00515054169548E-26,-1.1518563880486E-13,
-1.));
#22214=DIRECTION('ref_axis',(8.72635297355373E-14,-1.,1.1518563880486E-13));
#22215=DIRECTION('',(1.,8.72635297355373E-14,0.));
#22216=DIRECTION('',(8.72635297355373E-14,-1.,1.1518563880486E-13));
#22217=DIRECTION('',(-1.,-8.72635297355373E-14,0.));
#22218=DIRECTION('',(8.72635297355373E-14,-1.,1.1518563880486E-13));
#22219=DIRECTION('center_axis',(-6.12643539041984E-14,-6.12643539042085E-14,
-1.));
#22220=DIRECTION('ref_axis',(1.,7.86672314591538E-14,-6.09036630651514E-14));
#22221=DIRECTION('center_axis',(-8.72635297355373E-14,1.,-1.1518563880486E-13));
#22222=DIRECTION('ref_axis',(1.73003535575891E-29,-1.1518563880486E-13,
-1.));
#22223=DIRECTION('',(8.72635297355373E-14,-1.,1.1518563880486E-13));
#22224=DIRECTION('center_axis',(-4.42440467565883E-14,1.,-7.21582256614495E-14));
#22225=DIRECTION('ref_axis',(-1.,-4.31400946711492E-14,5.07530525542931E-15));
#22226=DIRECTION('center_axis',(8.1002659099073E-14,-1.,1.0891683800392E-13));
#22227=DIRECTION('ref_axis',(1.26882631385732E-15,-1.0911906299173E-13,
-1.));
#22228=DIRECTION('center_axis',(-1.,-8.72635297355373E-14,0.));
#22229=DIRECTION('ref_axis',(-8.72635297355373E-14,1.,-1.1518563880486E-13));
#22230=DIRECTION('',(-8.72635297355373E-14,1.,-1.1518563880486E-13));
#22231=DIRECTION('',(-1.00515054169548E-26,1.1518563880486E-13,1.));
#22232=DIRECTION('',(1.00515054169548E-26,-1.1518563880486E-13,-1.));
#22233=DIRECTION('center_axis',(-1.,-8.81911644086279E-14,-6.4214875247015E-16));
#22234=DIRECTION('ref_axis',(-8.81834288130837E-14,1.,0.));
#22235=DIRECTION('center_axis',(-8.72635297355373E-14,1.,-1.1518563880486E-13));
#22236=DIRECTION('ref_axis',(1.00515054169548E-26,-1.1518563880486E-13,
-1.));
#22237=DIRECTION('',(1.,8.72635297355373E-14,0.));
#22238=DIRECTION('',(1.00515054169548E-26,-1.1518563880486E-13,-1.));
#22239=DIRECTION('',(1.,8.72635297355373E-14,0.));
#22240=DIRECTION('center_axis',(-6.73907892946183E-14,-1.,6.73907892946096E-14));
#22241=DIRECTION('ref_axis',(1.,-6.85166209482953E-14,1.26882631385732E-13));
#22242=DIRECTION('',(-1.00515054169548E-26,1.1518563880486E-13,1.));
#22243=DIRECTION('',(-1.,-8.72635297355373E-14,0.));
#22244=DIRECTION('',(-1.00515054169548E-26,1.1518563880486E-13,1.));
#22245=DIRECTION('center_axis',(0.4999999999905,-5.61219244898395E-14,-0.866025403789923));
#22246=DIRECTION('ref_axis',(-0.866025403789923,-1.33165252976688E-13,-0.4999999999905));
#22247=DIRECTION('',(0.866025403789926,1.33165252976688E-13,0.499999999990495));
#22248=DIRECTION('',(8.72635297355373E-14,-1.,1.1518563880486E-13));
#22249=DIRECTION('',(-8.72635297355373E-14,1.,-1.1518563880486E-13));
#22250=DIRECTION('center_axis',(1.,8.72635297355373E-14,0.));
#22251=DIRECTION('ref_axis',(8.72635297355373E-14,-1.,1.1518563880486E-13));
#22252=DIRECTION('',(-1.00515054169548E-26,1.1518563880486E-13,1.));
#22253=DIRECTION('',(-8.72635297355373E-14,1.,-1.1518563880486E-13));
#22254=DIRECTION('center_axis',(0.4999999999905,1.43385454223719E-13,0.866025403789923));
#22255=DIRECTION('ref_axis',(0.866025403789923,1.79796141740169E-14,-0.4999999999905));
#22256=DIRECTION('',(-0.866025403789926,-1.79796141740178E-14,0.499999999990495));
#22257=DIRECTION('',(-8.72635297355373E-14,1.,-1.1518563880486E-13));
#22258=DIRECTION('center_axis',(-0.4999999999905,5.61219244898395E-14,0.866025403789923));
#22259=DIRECTION('ref_axis',(0.866025403789923,1.33165252976688E-13,0.4999999999905));
#22260=DIRECTION('',(-0.866025403789926,-1.33165252976688E-13,-0.499999999990495));
#22261=DIRECTION('',(-8.72635297355373E-14,1.,-1.1518563880486E-13));
#22262=DIRECTION('center_axis',(-1.,-8.72635297355373E-14,0.));
#22263=DIRECTION('ref_axis',(-8.72635297355373E-14,1.,-1.1518563880486E-13));
#22264=DIRECTION('',(1.00515054169548E-26,-1.1518563880486E-13,-1.));
#22265=DIRECTION('',(-8.72635297355373E-14,1.,-1.1518563880486E-13));
#22266=DIRECTION('center_axis',(-0.4999999999905,-1.43385454223719E-13,
-0.866025403789923));
#22267=DIRECTION('ref_axis',(-0.866025403789923,-1.79796141740169E-14,0.4999999999905));
#22268=DIRECTION('',(0.866025403789926,1.79796141740177E-14,-0.499999999990495));
#22269=DIRECTION('center_axis',(1.,8.72635297355373E-14,0.));
#22270=DIRECTION('ref_axis',(8.72635297355373E-14,-1.,1.1518563880486E-13));
#22271=DIRECTION('',(8.72635297355373E-14,-1.,1.1518563880486E-13));
#22272=DIRECTION('',(1.00515054169548E-26,-1.1518563880486E-13,-1.));
#22273=DIRECTION('',(8.72635297355373E-14,-1.,1.1518563880486E-13));
#22274=DIRECTION('center_axis',(1.,8.90883600993061E-14,2.80817075700403E-15));
#22275=DIRECTION('ref_axis',(-2.53765262771465E-15,4.82153999265783E-14,
1.));
#22276=DIRECTION('center_axis',(-8.72635297355373E-14,1.,-1.1518563880486E-13));
#22277=DIRECTION('ref_axis',(1.73003535575891E-29,-1.1518563880486E-13,
-1.));
#22278=DIRECTION('',(8.72635297355373E-14,-1.,1.1518563880486E-13));
#22279=DIRECTION('center_axis',(6.73907892946244E-14,1.,-6.73907892946245E-14));
#22280=DIRECTION('ref_axis',(-2.53765262771465E-15,-6.85166209482954E-14,
-1.));
#22281=DIRECTION('center_axis',(1.00515054169548E-26,-1.1518563880486E-13,
-1.));
#22282=DIRECTION('ref_axis',(8.72635297355373E-14,-1.,1.1518563880486E-13));
#22283=DIRECTION('',(-8.72635297355373E-14,1.,-1.1518563880486E-13));
#22284=DIRECTION('',(-1.,-8.72635297355373E-14,0.));
#22285=DIRECTION('center_axis',(7.35172246850504E-14,-7.35172246850366E-14,
-1.));
#22286=DIRECTION('ref_axis',(-8.62801893422977E-14,1.,-7.10542735760099E-14));
#22287=DIRECTION('center_axis',(-1.04744440165193E-14,-1.15185638804861E-13,
-1.));
#22288=DIRECTION('ref_axis',(-1.,-8.71698546678346E-14,1.04744440165294E-14));
#22289=DIRECTION('',(1.04744440165193E-14,1.15185638804861E-13,1.));
#22290=DIRECTION('',(-5.23722200825506E-15,-1.09948416796596E-13,-1.));
#22291=DIRECTION('center_axis',(2.66521584365477E-12,-5.1895433423456E-12,
1.));
#22292=DIRECTION('ref_axis',(0.707106781186605,-0.70710678118649,-5.55555601522426E-12));
#22293=DIRECTION('center_axis',(0.707106781186606,-0.707106781186489,7.40419959009745E-14));
#22294=DIRECTION('ref_axis',(-0.707106781186489,-0.707106781186606,8.14485462942204E-14));
#22295=DIRECTION('',(-1.04744440165193E-14,-1.15185638804861E-13,-1.));
#22296=DIRECTION('',(0.707106781186493,0.707106781186602,-8.95362847158453E-14));
#22297=DIRECTION('center_axis',(-1.04744440165193E-14,-1.15185638804861E-13,
-1.));
#22298=DIRECTION('ref_axis',(-1.,-8.71698546678346E-14,1.04744440165294E-14));
#22299=DIRECTION('',(-1.04744440165193E-14,-1.15185638804861E-13,-1.));
#22300=DIRECTION('center_axis',(4.57696995050001E-12,-2.23639690875147E-12,
1.));
#22301=DIRECTION('ref_axis',(0.986663993658371,-0.162770278669399,-4.88054041625221E-12));
#22302=DIRECTION('center_axis',(-1.04744440165193E-14,-1.15185638804861E-13,
-1.));
#22303=DIRECTION('ref_axis',(1.,9.24743105072028E-14,-1.047444401653E-14));
#22304=DIRECTION('',(-1.04744440165193E-14,-1.15185638804861E-13,-1.));
#22305=DIRECTION('center_axis',(1.67705924609206E-12,1.20380416834642E-13,
1.));
#22306=DIRECTION('ref_axis',(0.986663993658341,0.162770278669584,-1.67442661407532E-12));
#22307=DIRECTION('center_axis',(-1.04744440165193E-14,-1.15185638804861E-13,
-1.));
#22308=DIRECTION('ref_axis',(-1.,-8.72782748850831E-14,1.04744440165294E-14));
#22309=DIRECTION('',(-5.23722200825424E-15,-1.20422860813125E-13,-1.));
#22310=DIRECTION('center_axis',(4.86004852695852E-12,2.49599579008935E-12,
1.));
#22311=DIRECTION('ref_axis',(0.707106781186489,0.707106781186606,-5.20028464734421E-12));
#22312=DIRECTION('center_axis',(0.707106781186489,0.707106781186606,-8.88550966874672E-14));
#22313=DIRECTION('ref_axis',(0.707106781186606,-0.707106781186489,8.14485462942212E-14));
#22314=DIRECTION('',(-1.04744440165193E-14,-1.15185638804861E-13,-1.));
#22315=DIRECTION('',(-0.707106781186601,0.707106781186494,-7.33608078725965E-14));
#22316=DIRECTION('center_axis',(-1.04744440165193E-14,-1.15185638804861E-13,
-1.));
#22317=DIRECTION('ref_axis',(-1.,-8.71698546678346E-14,1.04744440165294E-14));
#22318=DIRECTION('',(-1.04744440165193E-14,-1.15185638804861E-13,-1.));
#22319=DIRECTION('center_axis',(3.04596096417561E-12,5.93090667696643E-12,
1.));
#22320=DIRECTION('ref_axis',(0.162770278669402,0.986663993658371,-6.34603480875743E-12));
#22321=DIRECTION('center_axis',(-1.04744440165193E-14,-1.15185638804861E-13,
-1.));
#22322=DIRECTION('ref_axis',(-1.,-8.72097194830903E-14,1.04744440165294E-14));
#22323=DIRECTION('',(-1.04744440165193E-14,-1.15185638804861E-13,-1.));
#22324=DIRECTION('center_axis',(-5.78383051437747E-13,7.50458952439442E-12,
1.));
#22325=DIRECTION('ref_axis',(-0.162770278669582,0.986663993658341,-7.49850197409643E-12));
#22326=DIRECTION('center_axis',(-1.04744440165193E-14,-1.15185638804861E-13,
-1.));
#22327=DIRECTION('ref_axis',(-1.,-8.71698546678346E-14,1.04744440165294E-14));
#22328=DIRECTION('',(-5.23722200825505E-15,-1.09948416796596E-13,-1.));
#22329=DIRECTION('center_axis',(-2.58060581687203E-12,5.02479593465201E-12,
1.));
#22330=DIRECTION('ref_axis',(-0.707106781186607,0.707106781186488,-5.37792033128426E-12));
#22331=DIRECTION('center_axis',(-0.707106781186605,0.70710678118649,-7.40419959009746E-14));
#22332=DIRECTION('ref_axis',(0.70710678118649,0.707106781186605,-8.14485462942203E-14));
#22333=DIRECTION('',(-1.04744440165193E-14,-1.15185638804861E-13,-1.));
#22334=DIRECTION('',(-0.707106781186489,-0.707106781186606,8.54924155050331E-14));
#22335=DIRECTION('center_axis',(-1.04744440165193E-14,-1.15185638804861E-13,
-1.));
#22336=DIRECTION('ref_axis',(-1.,-8.72782748850831E-14,1.04744440165294E-14));
#22337=DIRECTION('center_axis',(-5.63736932649778E-12,3.00942475177315E-12,
1.));
#22338=DIRECTION('ref_axis',(-0.986663993658371,0.162770278669398,-6.05293593025637E-12));
#22339=DIRECTION('center_axis',(-1.04744440165193E-14,-1.15185638804861E-13,
-1.));
#22340=DIRECTION('ref_axis',(-1.,-8.71698546678346E-14,1.04744440165294E-14));
#22341=DIRECTION('',(-5.23722200825426E-15,-1.20422860813125E-13,-1.));
#22342=DIRECTION('center_axis',(-5.68569950679339E-12,-2.8139702200907E-12,
1.));
#22343=DIRECTION('ref_axis',(-0.70710678118649,-0.707106781186605,-6.00852700927135E-12));
#22344=DIRECTION('center_axis',(-0.70710678118649,-0.707106781186605,8.88550966874671E-14));
#22345=DIRECTION('ref_axis',(-0.707106781186605,0.70710678118649,-8.14485462942213E-14));
#22346=DIRECTION('',(-1.04744440165193E-14,-1.15185638804861E-13,-1.));
#22347=DIRECTION('',(0.707106781186601,-0.707106781186494,7.74046770834091E-14));
#22348=DIRECTION('center_axis',(-1.04744440165193E-14,-1.15185638804861E-13,
-1.));
#22349=DIRECTION('ref_axis',(-1.,-8.71698546678346E-14,1.04744440165294E-14));
#22350=DIRECTION('',(-1.04744440165193E-14,-1.15185638804861E-13,-1.));
#22351=DIRECTION('center_axis',(-2.65628776850208E-12,-4.93387739816273E-12,
1.));
#22352=DIRECTION('ref_axis',(-0.162770278669406,-0.98666399365837,-5.30242516560978E-12));
#22353=DIRECTION('center_axis',(-1.04744440165193E-14,-1.15185638804861E-13,
-1.));
#22354=DIRECTION('ref_axis',(-1.,-8.72870330641923E-14,1.04744440165294E-14));
#22355=DIRECTION('center_axis',(6.31496326740432E-13,-7.26238032379499E-12,
1.));
#22356=DIRECTION('ref_axis',(0.162770278669577,-0.986663993658342,-7.26851571812066E-12));
#22357=DIRECTION('center_axis',(7.55724335745396E-14,-0.866025403780606,
-0.500000000006639));
#22358=DIRECTION('ref_axis',(4.36317648683479E-14,-0.500000000006639,0.866025403780606));
#22359=DIRECTION('',(-1.,-8.72635297355373E-14,0.));
#22360=DIRECTION('',(1.,8.72635297355373E-14,0.));
#22361=DIRECTION('center_axis',(7.55724335745396E-14,-0.866025403780606,
-0.500000000006639));
#22362=DIRECTION('ref_axis',(0.,-0.500000000006639,0.866025403780606));
#22363=DIRECTION('center_axis',(7.55724335745296E-14,-0.866025403780491,
0.500000000006838));
#22364=DIRECTION('ref_axis',(-4.36317648683653E-14,0.500000000006838,0.866025403780491));
#22365=DIRECTION('',(1.,8.72635297355373E-14,0.));
#22366=DIRECTION('center_axis',(7.55724335745296E-14,-0.866025403780491,
0.500000000006838));
#22367=DIRECTION('ref_axis',(0.,0.500000000006838,0.866025403780491));
#22368=DIRECTION('center_axis',(-1.00515054169548E-26,1.1518563880486E-13,
1.));
#22369=DIRECTION('ref_axis',(-8.72635297355373E-14,1.,-1.1518563880486E-13));
#22370=DIRECTION('',(1.,8.72635297355373E-14,0.));
#22371=DIRECTION('center_axis',(-2.00908022958255E-11,-2.95761452118009E-13,
1.));
#22372=DIRECTION('ref_axis',(0.989245507946394,0.146264571950559,1.99196012991554E-11));
#22373=DIRECTION('center_axis',(-7.55724335745396E-14,0.866025403780606,
0.500000000006639));
#22374=DIRECTION('ref_axis',(-4.36317648683479E-14,0.500000000006639,-0.866025403780606));
#22375=DIRECTION('',(1.,8.72635297355373E-14,0.));
#22376=DIRECTION('center_axis',(-7.55724335745396E-14,0.866025403780606,
0.500000000006639));
#22377=DIRECTION('ref_axis',(0.,0.500000000006639,-0.866025403780606));
#22378=DIRECTION('center_axis',(-7.55724335745296E-14,0.866025403780491,
-0.500000000006838));
#22379=DIRECTION('ref_axis',(4.36317648683653E-14,-0.500000000006838,-0.866025403780491));
#22380=DIRECTION('',(1.,8.72635297355373E-14,0.));
#22381=DIRECTION('center_axis',(-7.55724335745296E-14,0.866025403780491,
-0.500000000006838));
#22382=DIRECTION('ref_axis',(0.,-0.500000000006838,-0.866025403780491));
#22383=DIRECTION('center_axis',(1.00515054169548E-26,-1.1518563880486E-13,
-1.));
#22384=DIRECTION('ref_axis',(8.72635297355373E-14,-1.,1.1518563880486E-13));
#22385=DIRECTION('center_axis',(4.00087977969525E-12,-2.94175337366331E-13,
-1.));
#22386=DIRECTION('ref_axis',(0.989245507946313,-0.14626457195111,3.99976089707118E-12));
#22387=DIRECTION('center_axis',(7.55724335745396E-14,-0.866025403780606,
-0.500000000006639));
#22388=DIRECTION('ref_axis',(4.36317648683479E-14,-0.500000000006639,0.866025403780606));
#22389=DIRECTION('',(-1.,-8.72635297355373E-14,0.));
#22390=DIRECTION('',(1.,8.72635297355373E-14,0.));
#22391=DIRECTION('center_axis',(7.55724335745396E-14,-0.866025403780606,
-0.500000000006639));
#22392=DIRECTION('ref_axis',(0.,-0.500000000006639,0.866025403780606));
#22393=DIRECTION('center_axis',(7.55724335745296E-14,-0.866025403780491,
0.500000000006838));
#22394=DIRECTION('ref_axis',(-4.36317648683653E-14,0.500000000006838,0.866025403780491));
#22395=DIRECTION('',(1.,8.72635297355373E-14,0.));
#22396=DIRECTION('center_axis',(7.55724335745296E-14,-0.866025403780491,
0.500000000006838));
#22397=DIRECTION('ref_axis',(0.,0.500000000006838,0.866025403780491));
#22398=DIRECTION('center_axis',(-1.00515054169548E-26,1.1518563880486E-13,
1.));
#22399=DIRECTION('ref_axis',(-8.72635297355373E-14,1.,-1.1518563880486E-13));
#22400=DIRECTION('',(1.,8.72635297355373E-14,0.));
#22401=DIRECTION('center_axis',(3.33226641230312E-12,2.69627681862394E-13,
1.));
#22402=DIRECTION('ref_axis',(0.98924550794629,0.146264571951266,-3.33733424985186E-12));
#22403=DIRECTION('center_axis',(-7.55724335745396E-14,0.866025403780606,
0.500000000006639));
#22404=DIRECTION('ref_axis',(-4.36317648683479E-14,0.500000000006639,-0.866025403780606));
#22405=DIRECTION('',(1.,8.72635297355373E-14,0.));
#22406=DIRECTION('center_axis',(-7.55724335745396E-14,0.866025403780606,
0.500000000006639));
#22407=DIRECTION('ref_axis',(0.,0.500000000006639,-0.866025403780606));
#22408=DIRECTION('center_axis',(-7.55724335745296E-14,0.866025403780491,
-0.500000000006838));
#22409=DIRECTION('ref_axis',(4.36317648683653E-14,-0.500000000006838,-0.866025403780491));
#22410=DIRECTION('',(1.,8.72635297355373E-14,0.));
#22411=DIRECTION('center_axis',(-7.55724335745296E-14,0.866025403780491,
-0.500000000006838));
#22412=DIRECTION('ref_axis',(0.,-0.500000000006838,-0.866025403780491));
#22413=DIRECTION('center_axis',(1.00515054169548E-26,-1.1518563880486E-13,
-1.));
#22414=DIRECTION('ref_axis',(8.72635297355373E-14,-1.,1.1518563880486E-13));
#22415=DIRECTION('center_axis',(2.66725318646372E-12,-1.96116891577676E-13,
-1.));
#22416=DIRECTION('ref_axis',(0.989245507946304,-0.146264571951168,2.66770731298914E-12));
#22417=DIRECTION('center_axis',(1.00515054169548E-26,-1.1518563880486E-13,
-1.));
#22418=DIRECTION('ref_axis',(8.72318090776908E-14,-1.,1.1518563880486E-13));
#22419=DIRECTION('',(-1.00515054169548E-26,1.1518563880486E-13,1.));
#22420=DIRECTION('center_axis',(1.,8.72635297355373E-14,0.));
#22421=DIRECTION('ref_axis',(8.72635297355373E-14,-1.,1.18952466924124E-13));
#22422=DIRECTION('',(1.,8.72635297355373E-14,0.));
#22423=DIRECTION('center_axis',(8.72635297355373E-14,-1.,1.1518563880486E-13));
#22424=DIRECTION('ref_axis',(-1.00515054169548E-26,1.1518563880486E-13,
1.));
#22425=DIRECTION('center_axis',(8.49211903186698E-14,-1.,1.15553367270777E-13));
#22426=DIRECTION('ref_axis',(1.,8.37425367145833E-14,9.13554945977273E-14));
#22427=DIRECTION('',(1.,8.72635297355373E-14,0.));
#22428=DIRECTION('',(-1.00515054169548E-26,1.1518563880486E-13,1.));
#22429=DIRECTION('center_axis',(-1.00515054169548E-26,1.1518563880486E-13,
1.));
#22430=DIRECTION('ref_axis',(-8.72318090776908E-14,1.,-1.1518563880486E-13));
#22431=DIRECTION('',(1.00515054169548E-26,-1.1518563880486E-13,-1.));
#22432=DIRECTION('center_axis',(-8.72635297355373E-14,1.,-1.1518563880486E-13));
#22433=DIRECTION('ref_axis',(1.00515054169548E-26,-1.1518563880486E-13,
-1.));
#22434=DIRECTION('',(1.,8.72635297355373E-14,0.));
#22435=DIRECTION('center_axis',(8.71290944895014E-14,-1.,1.15043273394353E-13));
#22436=DIRECTION('ref_axis',(-1.26882631385732E-15,-1.14194368247158E-13,
-1.));
#22437=DIRECTION('',(1.00515054169548E-26,-1.1518563880486E-13,-1.));
#22438=DIRECTION('center_axis',(-8.72635297355373E-14,1.,-1.1518563880486E-13));
#22439=DIRECTION('ref_axis',(1.00515054169548E-26,-1.1518563880486E-13,
-1.));
#22440=DIRECTION('',(-1.,-8.72635297355373E-14,0.));
#22441=DIRECTION('center_axis',(8.2797050480443E-14,-1.,1.13248882013028E-13));
#22442=DIRECTION('ref_axis',(-1.26882631385733E-15,1.1419436824716E-13,
1.));
#22443=DIRECTION('',(-1.00515054169548E-26,1.1518563880486E-13,1.));
#22444=DIRECTION('center_axis',(1.,8.72635297355373E-14,0.));
#22445=DIRECTION('ref_axis',(8.72635297355373E-14,-1.,1.18952466924124E-13));
#22446=DIRECTION('',(-1.,-8.72635297355373E-14,0.));
#22447=DIRECTION('center_axis',(-8.72635297355373E-14,1.,-1.1518563880486E-13));
#22448=DIRECTION('ref_axis',(1.00515054169548E-26,-1.1518563880486E-13,
-1.));
#22449=DIRECTION('',(1.00515054169548E-26,-1.1518563880486E-13,-1.));
#22450=DIRECTION('center_axis',(-1.8379306171262E-14,-1.,1.83793061712636E-14));
#22451=DIRECTION('ref_axis',(-1.,1.77635683940026E-14,7.61295788314397E-14));
#22452=DIRECTION('',(-1.,-8.72635297355373E-14,0.));
#22453=DIRECTION('center_axis',(-0.86602540378448,0.499999999999929,-4.85216847935981E-14));
#22454=DIRECTION('ref_axis',(0.499999999999929,0.86602540378448,-9.9753689356147E-14));
#22455=DIRECTION('',(0.499999999999923,0.866025403784483,-1.06713055052629E-13));
#22456=DIRECTION('',(-1.04744440165193E-14,-1.15185638804861E-13,-1.));
#22457=DIRECTION('center_axis',(-1.04744440165193E-14,-1.15185638804861E-13,
-1.));
#22458=DIRECTION('ref_axis',(-1.,-8.72533584376409E-14,1.04744440165294E-14));
#22459=DIRECTION('center_axis',(-4.93888884645662E-14,-1.74996285159289E-13,
-1.));
#22460=DIRECTION('ref_axis',(-0.757843547050805,-0.652436325010689,1.51817826771104E-13));
#22461=DIRECTION('',(-2.61861100412291E-15,-1.10650071500444E-13,-1.));
#22462=DIRECTION('center_axis',(0.500000000000096,-0.866025403784383,9.4516467347881E-14));
#22463=DIRECTION('ref_axis',(-0.866025403784383,-0.500000000000096,5.75928194024323E-14));
#22464=DIRECTION('',(-0.866025403784382,-0.500000000000098,6.45521992358119E-14));
#22465=DIRECTION('center_axis',(-0.499999999999945,-0.866025403784471,1.04990911364411E-13));
#22466=DIRECTION('ref_axis',(-0.866025403784471,0.499999999999945,-5.75928194024323E-14));
#22467=DIRECTION('',(-0.866025403784468,0.499999999999948,-4.71542784478838E-14));
#22468=DIRECTION('',(-1.04744440165193E-14,-1.15185638804861E-13,-1.));
#22469=DIRECTION('center_axis',(-1.04744440165193E-14,-1.15185638804861E-13,
-1.));
#22470=DIRECTION('ref_axis',(-1.,-8.72533584376409E-14,1.04744440165294E-14));
#22471=DIRECTION('center_axis',(4.93888884646039E-14,-1.74996285159287E-13,
-1.));
#22472=DIRECTION('ref_axis',(0.652436325010704,-0.757843547050793,1.65057753524397E-13));
#22473=DIRECTION('',(-7.85583301238657E-15,-1.19721206109277E-13,-1.));
#22474=DIRECTION('center_axis',(0.866025403784393,0.50000000000008,-6.66639540112628E-14));
#22475=DIRECTION('ref_axis',(0.50000000000008,-0.866025403784393,9.9753689356147E-14));
#22476=DIRECTION('',(0.500000000000079,-0.866025403784393,9.62741799074761E-14));
#22477=DIRECTION('center_axis',(0.86602540378448,-0.499999999999929,4.85216847935981E-14));
#22478=DIRECTION('ref_axis',(-0.499999999999929,-0.86602540378448,9.9753689356147E-14));
#22479=DIRECTION('',(-0.49999999999993,-0.866025403784479,1.03233198804818E-13));
#22480=DIRECTION('',(-1.04744440165193E-14,-1.15185638804861E-13,-1.));
#22481=DIRECTION('center_axis',(-1.04744440165193E-14,-1.15185638804861E-13,
-1.));
#22482=DIRECTION('ref_axis',(-1.,-8.72533584376409E-14,1.04744440165294E-14));
#22483=DIRECTION('center_axis',(-5.77627149108745E-14,-1.66622458712969E-13,
-1.));
#22484=DIRECTION('ref_axis',(0.757843547050804,0.65243632501069,-1.52700488554662E-13));
#22485=DIRECTION('',(-2.61861100412291E-15,-1.10650071500444E-13,-1.));
#22486=DIRECTION('center_axis',(-0.500000000000096,0.866025403784383,-9.4516467347881E-14));
#22487=DIRECTION('ref_axis',(0.866025403784383,0.500000000000096,-5.75928194024323E-14));
#22488=DIRECTION('',(0.866025403784385,0.500000000000094,-6.80317109102609E-14));
#22489=DIRECTION('center_axis',(0.499999999999945,0.866025403784471,-1.04990911364411E-13));
#22490=DIRECTION('ref_axis',(0.866025403784471,-0.499999999999945,5.75928194024323E-14));
#22491=DIRECTION('',(0.86602540378447,-0.499999999999945,5.0632879163502E-14));
#22492=DIRECTION('',(-1.04744440165193E-14,-1.15185638804861E-13,-1.));
#22493=DIRECTION('center_axis',(-1.04744440165193E-14,-1.15185638804861E-13,
-1.));
#22494=DIRECTION('ref_axis',(-1.,-8.72533584376409E-14,1.04744440165294E-14));
#22495=DIRECTION('center_axis',(4.93888884645922E-14,-1.74996285159275E-13,
-1.));
#22496=DIRECTION('ref_axis',(-0.652436325010692,0.757843547050803,-1.65057753524405E-13));
#22497=DIRECTION('',(-7.85583301238656E-15,-1.19721206109277E-13,-1.));
#22498=DIRECTION('center_axis',(-0.866025403784393,-0.500000000000079,6.66639540112628E-14));
#22499=DIRECTION('ref_axis',(-0.500000000000079,0.866025403784393,-9.97536893561471E-14));
#22500=DIRECTION('',(-0.500000000000078,0.866025403784394,-9.27937835876813E-14));
#22501=DIRECTION('center_axis',(-1.04744440165193E-14,-1.15185638804861E-13,
-1.));
#22502=DIRECTION('ref_axis',(-1.,-8.72635297355361E-14,1.04744440165294E-14));
#22503=DIRECTION('center_axis',(1.14717457973843E-12,4.09170500797773E-13,
1.));
#22504=DIRECTION('ref_axis',(0.977277070396433,0.211965864415397,-1.20792265079108E-12));
#22505=DIRECTION('center_axis',(0.,0.,1.));
#22506=DIRECTION('ref_axis',(0.984863869999403,-0.173329621155183,0.));
#22507=DIRECTION('center_axis',(-4.47790050492473E-13,2.40527186556087E-12,
1.));
#22508=DIRECTION('ref_axis',(0.211965864415374,-0.977277070396437,2.44568809648228E-12));
#22509=DIRECTION('center_axis',(1.41284845480624E-12,7.19501758928192E-12,
1.));
#22510=DIRECTION('ref_axis',(-0.173329621155189,-0.984863869999402,7.33090625241919E-12));
#22511=DIRECTION('center_axis',(-2.39833919642918E-12,-4.70949484936173E-13,
1.));
#22512=DIRECTION('ref_axis',(-0.977277070396424,-0.211965864415433,-2.44379331585598E-12));
#22513=DIRECTION('center_axis',(-1.19362346291077E-11,2.54002290023133E-12,
1.));
#22514=DIRECTION('ref_axis',(-0.98486386999939,0.173329621155259,-1.21957555165768E-11));
#22515=DIRECTION('center_axis',(-1.05315117764831E-14,-2.7438796246474E-15,
1.));
#22516=DIRECTION('ref_axis',(-0.211965864415394,0.977277070396433,4.7369515717317E-16));
#22517=DIRECTION('center_axis',(1.00515054169548E-26,-1.1518563880486E-13,
-1.));
#22518=DIRECTION('ref_axis',(8.72635297355373E-14,-1.,1.1518563880486E-13));
#22519=DIRECTION('center_axis',(1.91944255730871E-14,-1.10978678768031E-13,
-1.));
#22520=DIRECTION('ref_axis',(1.,0.,1.95434151289614E-14));
#22521=DIRECTION('center_axis',(1.9194425573087E-14,-1.1097867876803E-13,
-1.));
#22522=DIRECTION('ref_axis',(1.,0.,1.95434151289613E-14));
#22523=DIRECTION('center_axis',(-8.72635297355373E-14,1.,-1.1518563880486E-13));
#22524=DIRECTION('ref_axis',(1.73003535575891E-29,-1.1518563880486E-13,
-1.));
#22525=DIRECTION('center_axis',(-8.71290944895063E-14,1.,-1.15043273394367E-13));
#22526=DIRECTION('ref_axis',(1.,8.6280189342298E-14,0.));
#22527=DIRECTION('',(8.72635297355373E-14,-1.,1.1518563880486E-13));
#22528=DIRECTION('',(-8.72635297355373E-14,1.,-1.1518563880486E-13));
#22529=DIRECTION('center_axis',(1.,8.72635297355373E-14,0.));
#22530=DIRECTION('ref_axis',(8.72635297355373E-14,-1.,1.1518563880486E-13));
#22531=DIRECTION('',(1.00515054169548E-26,-1.1518563880486E-13,-1.));
#22532=DIRECTION('',(8.72635297355373E-14,-1.,1.1518563880486E-13));
#22533=DIRECTION('center_axis',(-8.72635297355373E-14,1.,-1.1518563880486E-13));
#22534=DIRECTION('ref_axis',(1.73003535575891E-29,-1.1518563880486E-13,
-1.));
#22535=DIRECTION('center_axis',(-8.67155817000303E-14,1.,-1.11221323261711E-13));
#22536=DIRECTION('ref_axis',(-1.26882631385732E-15,-1.11656715619444E-13,
-1.));
#22537=DIRECTION('',(8.72635297355373E-14,-1.,1.1518563880486E-13));
#22538=DIRECTION('center_axis',(1.00515054169548E-26,-1.1518563880486E-13,
-1.));
#22539=DIRECTION('ref_axis',(8.72635297355373E-14,-1.,1.1518563880486E-13));
#22540=DIRECTION('',(-1.,-8.72635297355373E-14,0.));
#22541=DIRECTION('',(8.72635297355373E-14,-1.,1.1518563880486E-13));
#22542=DIRECTION('center_axis',(-8.72635297355373E-14,1.,-1.1518563880486E-13));
#22543=DIRECTION('ref_axis',(1.73003535575891E-29,-1.1518563880486E-13,
-1.));
#22544=DIRECTION('center_axis',(-8.27970504804384E-14,1.,-1.13248882013014E-13));
#22545=DIRECTION('ref_axis',(-1.,-8.37425367145831E-14,0.));
#22546=DIRECTION('',(8.72635297355373E-14,-1.,1.1518563880486E-13));
#22547=DIRECTION('center_axis',(-1.,-8.72635297355373E-14,0.));
#22548=DIRECTION('ref_axis',(-8.72635297355373E-14,1.,-1.1518563880486E-13));
#22549=DIRECTION('',(-1.00515054169548E-26,1.1518563880486E-13,1.));
#22550=DIRECTION('',(8.72635297355373E-14,-1.,1.1518563880486E-13));
#22551=DIRECTION('center_axis',(-8.72635297355373E-14,1.,-1.1518563880486E-13));
#22552=DIRECTION('ref_axis',(1.73003535575891E-29,-1.1518563880486E-13,
-1.));
#22553=DIRECTION('center_axis',(1.22528707808408E-14,1.,-1.22528707808409E-14));
#22554=DIRECTION('ref_axis',(0.,1.26882631385732E-14,1.));
#22555=DIRECTION('',(8.72635297355373E-14,-1.,1.1518563880486E-13));
#22556=DIRECTION('center_axis',(-1.00515054169548E-26,1.1518563880486E-13,
1.));
#22557=DIRECTION('ref_axis',(-8.72635297355373E-14,1.,-1.1518563880486E-13));
#22558=DIRECTION('',(1.,8.72635297355373E-14,0.));
#22559=DIRECTION('',(0.379745299517171,0.590960642274619,-0.711729602290775));
#22560=DIRECTION('',(-0.476347793731818,-0.412136157605333,0.776683054405812));
#22561=DIRECTION('',(0.590600287990408,0.380161574531733,-0.711806488503161));
#22562=DIRECTION('',(0.411815896436094,0.476626859392517,-0.776681726544511));
#22563=DIRECTION('center_axis',(-1.04744440165193E-14,-1.15185638804861E-13,
-1.));
#22564=DIRECTION('ref_axis',(-1.,-8.72635297355361E-14,1.04744440165294E-14));
#22565=DIRECTION('center_axis',(-8.48926851182745E-12,-3.34708584909148E-10,
1.));
#22566=DIRECTION('ref_axis',(-0.0249675486418349,-0.999688262167171,-3.34816203926024E-10));
#22567=DIRECTION('',(-0.100909211142278,-0.472292312794079,0.875646790882181));
#22568=DIRECTION('',(-0.0724190381853189,-0.456279544171757,0.886884694015365));
#22569=DIRECTION('center_axis',(-1.04744440165193E-14,-1.15185638804861E-13,
-1.));
#22570=DIRECTION('ref_axis',(-1.,-8.72635297355361E-14,1.04744440165294E-14));
#22571=DIRECTION('center_axis',(-2.29622482795222E-12,-2.87759861733811E-10,
1.));
#22572=DIRECTION('ref_axis',(-0.00756134748309062,-0.9999714126035,-2.8776898705888E-10));
#22573=DIRECTION('',(-0.0127111307240333,-0.450090627151626,0.892892409255433));
#22574=DIRECTION('',(0.0127111306191146,-0.450090672347739,0.892892386474397));
#22575=DIRECTION('center_axis',(-1.04744440165193E-14,-1.15185638804861E-13,
-1.));
#22576=DIRECTION('ref_axis',(-1.,-8.72635297355361E-14,1.04744440165294E-14));
#22577=DIRECTION('center_axis',(-1.69115474723865E-12,1.9183849313996E-10,
1.));
#22578=DIRECTION('ref_axis',(0.0100693168850478,-0.999949303143649,1.91845790211371E-10));
#22579=DIRECTION('',(0.0724190350594109,-0.456279674184686,0.886884627382266));
#22580=DIRECTION('',(0.100909204542893,-0.472292525389385,0.875646676976415));
#22581=DIRECTION('center_axis',(-1.04744440165193E-14,-1.15185638804861E-13,
-1.));
#22582=DIRECTION('ref_axis',(-1.,-8.72635297355361E-14,1.04744440165294E-14));
#22583=DIRECTION('center_axis',(4.60132114045041E-12,-1.67344966178724E-10,
1.));
#22584=DIRECTION('ref_axis',(0.0272919172742142,-0.999627506249952,-1.67408177429198E-10));
#22585=DIRECTION('center_axis',(-1.04744440165193E-14,-1.15185638804861E-13,
-1.));
#22586=DIRECTION('ref_axis',(-1.,-8.72635297355361E-14,1.04744440165294E-14));
#22587=DIRECTION('center_axis',(-0.845914384560533,-0.303272038408841,0.438696848305206));
#22588=DIRECTION('ref_axis',(0.194713288745752,-0.941418664629657,-0.275350019198703));
#22589=DIRECTION('center_axis',(-1.04744440165193E-14,-1.15185638804861E-13,
-1.));
#22590=DIRECTION('ref_axis',(-1.,-8.72635297355361E-14,1.04744440165294E-14));
#22591=DIRECTION('',(0.456351649509837,-0.0724173292173613,0.886847733502586));
#22592=DIRECTION('center_axis',(-1.04744440165193E-14,-1.15185638804861E-13,
-1.));
#22593=DIRECTION('ref_axis',(-1.,-8.72635297355361E-14,1.04744440165294E-14));
#22594=DIRECTION('',(0.450163801758523,-0.0127110352586768,0.892855520881719));
#22595=DIRECTION('',(0.450163801758538,0.0127110352589581,0.892855520881708));
#22596=DIRECTION('center_axis',(-1.04744440165193E-14,-1.15185638804861E-13,
-1.));
#22597=DIRECTION('ref_axis',(-1.,-8.72635297355361E-14,1.04744440165294E-14));
#22598=DIRECTION('',(0.45635164950983,0.0724173292176335,0.886847733502568));
#22599=DIRECTION('',(0.472361792915589,0.100907068159402,0.875609559215204));
#22600=DIRECTION('center_axis',(0.00208426357814304,-0.478871212227244,
0.877882690309671));
#22601=DIRECTION('ref_axis',(0.261186023449167,0.84767244816946,0.461771893654439));
#22602=DIRECTION('center_axis',(1.04744440165193E-14,1.15185638804861E-13,
1.));
#22603=DIRECTION('ref_axis',(1.,8.72635297355361E-14,-1.04744440165294E-14));
#22604=DIRECTION('center_axis',(1.02694929293583E-14,1.15185638804861E-13,
1.));
#22605=DIRECTION('ref_axis',(1.,8.72362563773224E-14,-1.02694929293684E-14));
#22606=DIRECTION('',(0.368107017006031,0.529525460520388,0.764264359166115));
#22607=DIRECTION('',(0.215658660878526,0.571281776348565,0.79191443603467));
#22608=DIRECTION('center_axis',(1.04744440165193E-14,1.15185638804861E-13,
1.));
#22609=DIRECTION('ref_axis',(1.,8.72635297355361E-14,-1.04744440165294E-14));
#22610=DIRECTION('center_axis',(1.02694929293583E-14,1.15185638804861E-13,
1.));
#22611=DIRECTION('ref_axis',(1.,8.72362563773224E-14,-1.02694929293684E-14));
#22612=DIRECTION('',(0.111788425215345,0.585178590638193,0.803162103841168));
#22613=DIRECTION('',(-0.111788300989806,0.585180930864035,0.803160416053302));
#22614=DIRECTION('center_axis',(1.04744440165193E-14,1.15185638804861E-13,
1.));
#22615=DIRECTION('ref_axis',(1.,8.72635297355361E-14,-1.04744440165294E-14));
#22616=DIRECTION('center_axis',(1.02695629360633E-14,1.15185638804861E-13,
1.));
#22617=DIRECTION('ref_axis',(1.,8.72362563773224E-14,-1.02695629360733E-14));
#22618=DIRECTION('',(-0.215658204214253,0.571287278227592,0.791910591348792));
#22619=DIRECTION('',(-0.368105810341799,0.529534956436002,0.764258360965014));
#22620=DIRECTION('center_axis',(1.04744440165193E-14,1.15185638804861E-13,
1.));
#22621=DIRECTION('ref_axis',(1.,8.72635297355361E-14,-1.04744440165294E-14));
#22622=DIRECTION('center_axis',(1.02695629360633E-14,1.15185638804861E-13,
1.));
#22623=DIRECTION('ref_axis',(1.,8.72362563773224E-14,-1.02695629360733E-14));
#22624=DIRECTION('',(0.379787668322238,-0.590832026048182,-0.711813770579185));
#22625=DIRECTION('',(0.476375308922749,-0.412016801957993,-0.77672950243509));
#22626=DIRECTION('center_axis',(-0.000653357528254759,0.000583642099734136,
0.999999616242846));
#22627=DIRECTION('ref_axis',(-0.831134725976919,0.556070422329433,-0.000867574572038));
#22628=DIRECTION('center_axis',(-1.04744440165193E-14,-1.15185638804861E-13,
-1.));
#22629=DIRECTION('ref_axis',(-1.,-8.72635297355361E-14,1.04744440165294E-14));
#22630=DIRECTION('center_axis',(1.04599037721437E-14,1.17366013112296E-13,
1.));
#22631=DIRECTION('ref_axis',(1.,8.72640651830633E-14,-1.0459903772154E-14));
#22632=DIRECTION('center_axis',(-1.04744440165193E-14,-1.15185638804861E-13,
-1.));
#22633=DIRECTION('ref_axis',(-1.,-8.72635297355361E-14,1.04744440165294E-14));
#22634=DIRECTION('center_axis',(1.04599037721437E-14,1.17366013112296E-13,
1.));
#22635=DIRECTION('ref_axis',(1.,8.72640651830633E-14,-1.0459903772154E-14));
#22636=DIRECTION('center_axis',(1.04675235693219E-6,-2.73632311340696E-8,
-0.999999999999452));
#22637=DIRECTION('ref_axis',(0.995602221707021,-0.0936814609778925,1.04471240189441E-6));
#22638=DIRECTION('',(-0.472240244388769,0.100910816440637,0.87567468771509));
#22639=DIRECTION('',(-0.456226081184184,0.0724203048515813,0.886912093892358));
#22640=DIRECTION('center_axis',(-1.04744440165193E-14,-1.15185638804861E-13,
-1.));
#22641=DIRECTION('ref_axis',(-1.,-8.72635297355361E-14,1.04744440165294E-14));
#22642=DIRECTION('center_axis',(1.04599037721437E-14,1.17366013112296E-13,
1.));
#22643=DIRECTION('ref_axis',(1.,8.72640651830633E-14,-1.0459903772154E-14));
#22644=DIRECTION('',(-0.450036916879799,0.0127112008260562,0.892919480590991));
#22645=DIRECTION('',(-0.450037561084516,-0.0127111996490203,0.892919155924311));
#22646=DIRECTION('center_axis',(-1.04744440165193E-14,-1.15185638804861E-13,
-1.));
#22647=DIRECTION('ref_axis',(-1.,-8.72635297355361E-14,1.04744440165294E-14));
#22648=DIRECTION('center_axis',(1.04599037721437E-14,1.17366013112296E-13,
1.));
#22649=DIRECTION('ref_axis',(1.,8.72640651830633E-14,-1.0459903772154E-14));
#22650=DIRECTION('',(-0.456227934233452,-0.0724202606201595,0.886911144296195));
#22651=DIRECTION('',(-0.472243274438807,-0.100910722705367,0.875673064442657));
#22652=DIRECTION('center_axis',(-8.72635297355373E-14,1.,-1.1518563880486E-13));
#22653=DIRECTION('ref_axis',(1.00515054169548E-26,-1.1518563880486E-13,
-1.));
#22654=DIRECTION('',(1.,8.72635297355373E-14,0.));
#22655=DIRECTION('center_axis',(8.72635297355373E-14,-1.,1.1518563880486E-13));
#22656=DIRECTION('ref_axis',(6.05512374515433E-29,-1.1518563880486E-13,
-1.));
#22657=DIRECTION('',(1.00515054169548E-26,-1.1518563880486E-13,-1.));
#22658=DIRECTION('center_axis',(8.72635297355373E-14,-1.,1.1518563880486E-13));
#22659=DIRECTION('ref_axis',(6.05512374515433E-29,-1.1518563880486E-13,
-1.));
#22660=DIRECTION('',(-1.,-8.72635297355373E-14,0.));
#22661=DIRECTION('center_axis',(8.72635297355373E-14,-1.,1.1518563880486E-13));
#22662=DIRECTION('ref_axis',(6.05512374515433E-29,-1.1518563880486E-13,
-1.));
#22663=DIRECTION('',(-1.00515054169548E-26,1.1518563880486E-13,1.));
#22664=DIRECTION('center_axis',(8.72635297355373E-14,-1.,1.1518563880486E-13));
#22665=DIRECTION('ref_axis',(6.05512374515433E-29,-1.1518563880486E-13,
-1.));
#22666=DIRECTION('center_axis',(9.95715680553083E-15,1.12696349603476E-13,
1.));
#22667=DIRECTION('ref_axis',(1.,8.71251220484807E-14,-9.95715680554065E-15));
#22668=DIRECTION('center_axis',(9.95715680553083E-15,1.12696349603476E-13,
1.));
#22669=DIRECTION('ref_axis',(1.,8.71251220484807E-14,-9.95715680554065E-15));
#22670=DIRECTION('',(-0.0174340345131866,-0.000800581691362652,0.999847695156391));
#22671=DIRECTION('',(0.0130759035045374,0.0115588597183791,-0.999847695156393));
#22672=DIRECTION('center_axis',(1.06503951930529E-14,1.15185638804861E-13,
1.));
#22673=DIRECTION('ref_axis',(1.,8.72606242522541E-14,-1.06503951930629E-14));
#22674=DIRECTION('center_axis',(1.06503951930529E-14,1.15185638804861E-13,
1.));
#22675=DIRECTION('ref_axis',(1.,8.72606242522541E-14,-1.06503951930629E-14));
#22676=DIRECTION('',(0.0115565367885269,0.0130779565645496,-0.999847695156393));
#22677=DIRECTION('center_axis',(1.12018012904865E-14,1.15185638804861E-13,
1.));
#22678=DIRECTION('ref_axis',(1.,8.71251211483066E-14,-1.12018012904966E-14));
#22679=DIRECTION('center_axis',(1.12018012904865E-14,1.15185638804861E-13,
1.));
#22680=DIRECTION('ref_axis',(1.,8.71251211483066E-14,-1.12018012904966E-14));
#22681=DIRECTION('',(0.000800462344174388,0.0174340399931744,-0.999847695156393));
#22682=DIRECTION('center_axis',(1.04599037500094E-14,1.15185638804861E-13,
1.));
#22683=DIRECTION('ref_axis',(1.,8.72149721128382E-14,-1.04599037500194E-14));
#22684=DIRECTION('',(-0.000800509149934771,0.0174340378440839,-0.999847695156393));
#22685=DIRECTION('center_axis',(1.04599037500094E-14,1.15185638804861E-13,
1.));
#22686=DIRECTION('ref_axis',(1.,8.72149721128382E-14,-1.04599037500194E-14));
#22687=DIRECTION('center_axis',(1.12018011379709E-14,1.15185638804861E-13,
1.));
#22688=DIRECTION('ref_axis',(1.,8.71251199620744E-14,-1.1201801137981E-14));
#22689=DIRECTION('center_axis',(1.12018011379709E-14,1.15185638804861E-13,
1.));
#22690=DIRECTION('ref_axis',(1.,8.71251199620744E-14,-1.1201801137981E-14));
#22691=DIRECTION('',(-0.0115568680204753,0.0130776638589093,-0.999847695156393));
#22692=DIRECTION('center_axis',(1.06503951254365E-14,1.15185638804861E-13,
1.));
#22693=DIRECTION('ref_axis',(1.,8.72606236982606E-14,-1.06503951254465E-14));
#22694=DIRECTION('center_axis',(1.06503951254365E-14,1.15185638804861E-13,
1.));
#22695=DIRECTION('ref_axis',(1.,8.72606236982606E-14,-1.06503951254465E-14));
#22696=DIRECTION('',(-0.0130765548702522,0.0115581228222826,-0.999847695156392));
#22697=DIRECTION('center_axis',(9.957156389593E-15,1.18919572450962E-13,
1.));
#22698=DIRECTION('ref_axis',(1.,8.71251184090297E-14,-9.95715638960336E-15));
#22699=DIRECTION('center_axis',(9.957156389593E-15,1.18919572450962E-13,
1.));
#22700=DIRECTION('ref_axis',(1.,8.71251184090297E-14,-9.95715638960336E-15));
#22701=DIRECTION('center_axis',(9.95715638959301E-15,1.18919572450962E-13,
1.));
#22702=DIRECTION('ref_axis',(1.,8.72806989776172E-14,-9.95715638960339E-15));
#22703=DIRECTION('center_axis',(9.95715638959301E-15,1.18919572450962E-13,
1.));
#22704=DIRECTION('ref_axis',(1.,8.72806989776172E-14,-9.95715638960339E-15));
#22705=DIRECTION('',(-0.0130765548702503,-0.0115581228225151,-0.99984769515639));
#22706=DIRECTION('center_axis',(1.03276558792108E-14,1.15185638804861E-13,
1.));
#22707=DIRECTION('ref_axis',(1.,8.72606236982606E-14,-1.03276558792209E-14));
#22708=DIRECTION('center_axis',(1.03276558792108E-14,1.15185638804861E-13,
1.));
#22709=DIRECTION('ref_axis',(1.,8.72606236982606E-14,-1.03276558792209E-14));
#22710=DIRECTION('',(-0.0115163028275352,-0.0131134000030443,-0.99984769515639));
#22711=DIRECTION('center_axis',(1.01544784648356E-14,1.16878051882335E-13,
1.));
#22712=DIRECTION('ref_axis',(1.,8.72650493072682E-14,-1.01544784648458E-14));
#22713=DIRECTION('center_axis',(1.01544784648356E-14,1.16878051882335E-13,
1.));
#22714=DIRECTION('ref_axis',(1.,8.72650493072682E-14,-1.01544784648458E-14));
#22715=DIRECTION('center_axis',(1.02695629360633E-14,1.15185638804861E-13,
1.));
#22716=DIRECTION('ref_axis',(1.,8.72912849566231E-14,-1.02695629360733E-14));
#22717=DIRECTION('',(0.00366432240577321,-0.0170633886365656,-0.999847695156389));
#22718=DIRECTION('center_axis',(1.02695629360633E-14,1.15185638804861E-13,
1.));
#22719=DIRECTION('ref_axis',(1.,8.72912849566231E-14,-1.02695629360733E-14));
#22720=DIRECTION('center_axis',(9.30827207959047E-15,1.12647019146788E-13,
1.));
#22721=DIRECTION('ref_axis',(1.,8.72650507462529E-14,-9.3082720796003E-15));
#22722=DIRECTION('center_axis',(9.30827207959047E-15,1.12647019146788E-13,
1.));
#22723=DIRECTION('ref_axis',(1.,8.72650507462529E-14,-9.3082720796003E-15));
#22724=DIRECTION('',(0.0115164418467348,-0.013113277913841,-0.99984769515639));
#22725=DIRECTION('center_axis',(1.03276559454674E-14,1.15185638804861E-13,
1.));
#22726=DIRECTION('ref_axis',(1.,8.7260624258077E-14,-1.03276559454775E-14));
#22727=DIRECTION('center_axis',(1.03276559454674E-14,1.15185638804861E-13,
1.));
#22728=DIRECTION('ref_axis',(1.,8.7260624258077E-14,-1.03276559454775E-14));
#22729=DIRECTION('',(0.0130759007521692,-0.0115588628322128,-0.99984769515639));
#22730=DIRECTION('center_axis',(1.12018014099246E-14,1.11451705001549E-13,
1.));
#22731=DIRECTION('ref_axis',(1.,8.72807026524047E-14,-1.12018014099343E-14));
#22732=DIRECTION('center_axis',(1.12018014099246E-14,1.11451705001549E-13,
1.));
#22733=DIRECTION('ref_axis',(1.,8.72807026524047E-14,-1.12018014099343E-14));
#22734=DIRECTION('',(0.0174340340546429,-0.000800591677104543,-0.999847695156391));
#22735=DIRECTION('center_axis',(1.04599037721437E-14,1.17366013112296E-13,
1.));
#22736=DIRECTION('ref_axis',(-0.999999999999959,2.86379829728456E-7,1.04598701608845E-14));
#22737=DIRECTION('center_axis',(1.04599037721437E-14,1.17366013112296E-13,
1.));
#22738=DIRECTION('ref_axis',(1.,8.72628521386072E-14,-1.0459903772154E-14));
#22739=DIRECTION('center_axis',(-1.00515054169548E-26,1.1518563880486E-13,
1.));
#22740=DIRECTION('ref_axis',(-8.72635297355373E-14,1.,-1.1518563880486E-13));
#22741=DIRECTION('',(8.72635297355373E-14,-1.,1.1518563880486E-13));
#22742=DIRECTION('',(-8.72635297355373E-14,1.,-1.1518563880486E-13));
#22743=DIRECTION('',(-1.,-8.72635297355373E-14,0.));
#22744=DIRECTION('center_axis',(1.,8.72635297355373E-14,0.));
#22745=DIRECTION('ref_axis',(8.72635297355373E-14,-1.,1.1518563880486E-13));
#22746=DIRECTION('',(8.72635297355373E-14,-1.,1.1518563880486E-13));
#22747=DIRECTION('',(-8.72635297355373E-14,1.,-1.1518563880486E-13));
#22748=DIRECTION('',(-1.00515054169548E-26,1.1518563880486E-13,1.));
#22749=DIRECTION('center_axis',(-8.72635297355373E-14,1.,-1.1518563880486E-13));
#22750=DIRECTION('ref_axis',(6.05512374515433E-29,-1.1518563880486E-13,
-1.));
#22751=DIRECTION('center_axis',(-8.72635297355373E-14,1.,-1.1518563880486E-13));
#22752=DIRECTION('ref_axis',(6.05512374515433E-29,-1.1518563880486E-13,
-1.));
#22753=DIRECTION('center_axis',(1.00515054169548E-26,-1.1518563880486E-13,
-1.));
#22754=DIRECTION('ref_axis',(8.72635297355373E-14,-1.,1.1518563880486E-13));
#22755=DIRECTION('',(8.72635297355373E-14,-1.,1.1518563880486E-13));
#22756=DIRECTION('',(-8.72635297355373E-14,1.,-1.1518563880486E-13));
#22757=DIRECTION('',(1.,8.72635297355373E-14,0.));
#22758=DIRECTION('center_axis',(-8.72635297355373E-14,1.,-1.1518563880486E-13));
#22759=DIRECTION('ref_axis',(6.05512374515433E-29,-1.1518563880486E-13,
-1.));
#22760=DIRECTION('center_axis',(-8.72635297355373E-14,1.,-1.1518563880486E-13));
#22761=DIRECTION('ref_axis',(6.05512374515433E-29,-1.1518563880486E-13,
-1.));
#22762=DIRECTION('center_axis',(-8.72635297355373E-14,1.,-1.1518563880486E-13));
#22763=DIRECTION('ref_axis',(6.05512374515433E-29,-1.1518563880486E-13,
-1.));
#22764=DIRECTION('center_axis',(-8.72635297355373E-14,1.,-1.1518563880486E-13));
#22765=DIRECTION('ref_axis',(6.05512374515433E-29,-1.1518563880486E-13,
-1.));
#22766=DIRECTION('',(8.72635297355373E-14,-1.,1.1518563880486E-13));
#22767=DIRECTION('center_axis',(-8.72635297355373E-14,1.,-1.1518563880486E-13));
#22768=DIRECTION('ref_axis',(6.05512374515433E-29,-1.1518563880486E-13,
-1.));
#22769=DIRECTION('',(-8.72635297355373E-14,1.,-1.1518563880486E-13));
#22770=DIRECTION('center_axis',(-8.72635297355373E-14,1.,-1.1518563880486E-13));
#22771=DIRECTION('ref_axis',(6.05512374515433E-29,-1.1518563880486E-13,
-1.));
#22772=DIRECTION('center_axis',(-1.,-8.72635297355373E-14,0.));
#22773=DIRECTION('ref_axis',(-8.72635297355373E-14,1.,-1.1518563880486E-13));
#22774=DIRECTION('',(1.00515054169548E-26,-1.1518563880486E-13,-1.));
#22775=DIRECTION('',(-0.581868005306999,0.0361272616194947,0.812480427682988));
#22776=DIRECTION('center_axis',(-0.706995946343866,-0.707002335908082,-0.0174478902408474));
#22777=DIRECTION('ref_axis',(-0.485490346420283,0.503130085971089,-0.714954012593424));
#22778=DIRECTION('center_axis',(1.01785891439412E-10,1.01653359675599E-10,
-1.));
#22779=DIRECTION('ref_axis',(-0.707106780085371,0.707106782287724,-9.37138848923848E-14));
#22780=DIRECTION('',(0.0361272616297709,-0.581868005321186,0.81248042767237));
#22781=DIRECTION('center_axis',(-0.707002336415719,-0.70699594584904,-0.0174478897215777));
#22782=DIRECTION('ref_axis',(0.514376723468753,-0.497136627511086,-0.698764452401848));
#22783=DIRECTION('',(0.0361272616182702,0.581868005288873,-0.812480427696024));
#22784=DIRECTION('center_axis',(-0.707002329658505,0.706995952382432,0.0174478987934091));
#22785=DIRECTION('ref_axis',(-0.514376732675718,-0.497136618246221,-0.698764452215883));
#22786=DIRECTION('',(-0.581868005317437,-0.0361272616345021,-0.812480427674845));
#22787=DIRECTION('center_axis',(-4.27803755150032E-11,4.26274542481757E-11,
-1.));
#22788=DIRECTION('ref_axis',(0.707106783659767,0.707106778713328,-1.08131875993609E-13));
#22789=DIRECTION('center_axis',(0.706995945311992,-0.707002336973518,-0.0174478888805456));
#22790=DIRECTION('ref_axis',(0.497136628295254,0.514376722639527,-0.698764452454363));
#22791=DIRECTION('',(-0.58186800529869,0.0361272616310885,-0.812480427688423));
#22792=DIRECTION('center_axis',(-0.706984234058496,-0.707014463525137,0.0174310401004826));
#22793=DIRECTION('ref_axis',(0.497157132168199,-0.514363398390198,-0.698759672799438));
#22794=DIRECTION('',(0.0361272616460507,-0.581868005335907,-0.812480427661104));
#22795=DIRECTION('center_axis',(8.98778795138279E-11,8.97351529997424E-11,
-1.));
#22796=DIRECTION('ref_axis',(-0.707106777512622,0.707106784860473,-1.00922226080033E-13));
#22797=DIRECTION('center_axis',(-4.3591368164562E-11,-5.61674536871897E-11,
-1.));
#22798=DIRECTION('ref_axis',(0.78941644366153,-0.613858027948469,6.70995244962243E-14));
#22799=DIRECTION('center_axis',(0.707006995355329,0.706991448016083,-0.0174413574801738));
#22800=DIRECTION('ref_axis',(-0.513636500710189,0.496382763560557,-0.699844052041721));
#22801=DIRECTION('center_axis',(1.99622914093862E-10,-2.721998042675E-10,
-1.));
#22802=DIRECTION('ref_axis',(0.789416439455461,0.613858033357439,-9.50642645022728E-12));
#22803=DIRECTION('',(0.0361272616208185,0.581868005208879,0.812480427753199));
#22804=DIRECTION('center_axis',(-0.707006955053561,0.706991486952665,-0.0174414128542213));
#22805=DIRECTION('ref_axis',(0.501153812357023,0.483458857880451,-0.717713305642965));
#22806=DIRECTION('center_axis',(2.27115393216186E-10,-2.14586044118155E-10,
-1.));
#22807=DIRECTION('ref_axis',(0.707106783402892,0.707106778970203,8.85958869003344E-12));
#22808=DIRECTION('',(-0.581868005296781,-0.0361272616296084,0.812480427689856));
#22809=DIRECTION('center_axis',(-0.706995952053428,0.70700232999654,-0.0174478984273346));
#22810=DIRECTION('ref_axis',(-0.497136618691357,-0.514376732281121,-0.698764452189664));
#22811=DIRECTION('center_axis',(-1.04744440165193E-14,-1.15185638804861E-13,
-1.));
#22812=DIRECTION('ref_axis',(-1.,-8.72635297355361E-14,1.04744440165294E-14));
#22813=DIRECTION('center_axis',(1.20840226997713E-14,1.16284186323023E-13,
1.));
#22814=DIRECTION('ref_axis',(1.,8.73461657600799E-14,-1.20840226997814E-14));
#22815=DIRECTION('center_axis',(1.09854751816067E-14,1.15185638804861E-13,
1.));
#22816=DIRECTION('ref_axis',(1.,8.73461657600583E-14,-1.09854751816168E-14));
#22817=DIRECTION('center_axis',(1.04854396770053E-14,1.15185638804861E-13,
1.));
#22818=DIRECTION('ref_axis',(1.,8.72173693231828E-14,-1.04854396770154E-14));
#22819=DIRECTION('center_axis',(1.09854751816067E-14,1.15185638804861E-13,
1.));
#22820=DIRECTION('ref_axis',(1.,8.73461657600581E-14,-1.09854751816168E-14));
#22821=DIRECTION('center_axis',(9.88692766344469E-15,1.18481281359346E-13,
1.));
#22822=DIRECTION('ref_axis',(1.,8.73461657600578E-14,-9.88692766345504E-15));
#22823=DIRECTION('center_axis',(1.04854396770055E-14,1.1301218632279E-13,
1.));
#22824=DIRECTION('ref_axis',(1.,8.72632848014737E-14,-1.04854396770154E-14));
#22825=DIRECTION('center_axis',(1.09854751816069E-14,1.14087091286699E-13,
1.));
#22826=DIRECTION('ref_axis',(1.,8.72061879303152E-14,-1.09854751816168E-14));
#22827=DIRECTION('center_axis',(1.03092138003362E-14,1.18357704589583E-13,
1.));
#22828=DIRECTION('ref_axis',(1.,8.72387369821193E-14,-1.03092138003465E-14));
#22829=DIRECTION('center_axis',(1.06396373193144E-14,1.15185638804861E-13,
1.));
#22830=DIRECTION('ref_axis',(1.,8.72773155181867E-14,-1.06396373193244E-14));
#22831=DIRECTION('center_axis',(1.03092138003367E-14,1.135996059125E-13,
1.));
#22832=DIRECTION('ref_axis',(1.,8.72387369821196E-14,-1.03092138003466E-14));
#22833=DIRECTION('center_axis',(9.88692766344536E-15,1.12988543768537E-13,
1.));
#22834=DIRECTION('ref_axis',(1.,8.72061879303152E-14,-9.88692766345521E-15));
#22835=DIRECTION('center_axis',(8.72635297355373E-14,-1.,1.1518563880486E-13));
#22836=DIRECTION('ref_axis',(-1.00515054169548E-26,1.1518563880486E-13,
1.));
#22837=DIRECTION('',(0.499999999980758,-5.61219244913375E-14,-0.866025403795548));
#22838=DIRECTION('',(-0.499999999980758,-1.43385454223517E-13,-0.866025403795548));
#22839=DIRECTION('',(-1.,-8.72635297355373E-14,0.));
#22840=DIRECTION('',(-0.499999999980758,5.61219244913375E-14,0.866025403795548));
#22841=DIRECTION('',(0.499999999980758,1.43385454223517E-13,0.866025403795548));
#22842=DIRECTION('',(1.,8.72635297355373E-14,0.));
#22843=DIRECTION('center_axis',(8.72635297355373E-14,-1.,1.1518563880486E-13));
#22844=DIRECTION('ref_axis',(-1.00515054169548E-26,1.1518563880486E-13,
1.));
#22845=DIRECTION('',(0.499999999980758,-5.61219244913375E-14,-0.866025403795548));
#22846=DIRECTION('',(-0.499999999980758,-1.43385454223517E-13,-0.866025403795548));
#22847=DIRECTION('',(-1.,-8.72635297355373E-14,0.));
#22848=DIRECTION('',(-0.499999999980758,5.61219244913375E-14,0.866025403795548));
#22849=DIRECTION('',(0.499999999980758,1.43385454223517E-13,0.866025403795548));
#22850=DIRECTION('',(1.,8.72635297355373E-14,0.));
#22851=DIRECTION('center_axis',(1.,8.72635297355373E-14,0.));
#22852=DIRECTION('ref_axis',(8.72635297355373E-14,-1.,1.11022302462516E-13));
#22853=DIRECTION('',(1.,8.72635297355373E-14,0.));
#22854=DIRECTION('center_axis',(-1.00515054169548E-26,1.1518563880486E-13,
1.));
#22855=DIRECTION('ref_axis',(-9.02056207507939E-14,1.,-1.1518563880486E-13));
#22856=DIRECTION('',(1.00515054169548E-26,-1.1518563880486E-13,-1.));
#22857=DIRECTION('center_axis',(1.,8.72635297355373E-14,0.));
#22858=DIRECTION('ref_axis',(8.72635297355373E-14,-1.,1.11022302462516E-13));
#22859=DIRECTION('',(-1.,-8.72635297355373E-14,0.));
#22860=DIRECTION('center_axis',(-1.00515054169548E-26,1.1518563880486E-13,
1.));
#22861=DIRECTION('ref_axis',(-9.02056207507939E-14,1.,-1.1518563880486E-13));
#22862=DIRECTION('',(-1.00515054169548E-26,1.1518563880486E-13,1.));
#22863=DIRECTION('center_axis',(9.88692766344469E-15,1.18481281359346E-13,
1.));
#22864=DIRECTION('ref_axis',(1.,8.73345276938528E-14,-9.88692766345504E-15));
#22865=DIRECTION('center_axis',(9.88692766344469E-15,1.18481281359346E-13,
1.));
#22866=DIRECTION('ref_axis',(1.,8.73345276938528E-14,-9.88692766345504E-15));
#22867=DIRECTION('',(-0.0174340297464267,-0.000800685488963285,0.999847695156391));
#22868=DIRECTION('center_axis',(-0.998896061698716,0.0436127439212717,-0.0174524064372782));
#22869=DIRECTION('ref_axis',(0.0436193873652447,0.999048221581862,-1.1507597159015E-13));
#22870=DIRECTION('',(0.0177702355175903,0.00691046665269606,-0.999818215567356));
#22871=DIRECTION('',(-0.0436193873652537,-0.999048221581861,1.15076007599765E-13));
#22872=DIRECTION('center_axis',(-0.706999085398757,-0.706999085398894,-0.0174524064371947));
#22873=DIRECTION('ref_axis',(-0.707106781186615,0.70710678118648,-8.14490323933116E-14));
#22874=DIRECTION('',(0.00691046665279671,0.0177702355174836,-0.999818215567357));
#22875=DIRECTION('',(0.707106781186617,-0.707106781186478,7.26836276787581E-14));
#22876=DIRECTION('center_axis',(0.043612743921459,-0.99889606169871,-0.017452406437169));
#22877=DIRECTION('ref_axis',(-0.999048221581854,-0.04361938736543,5.02432903970128E-15));
#22878=DIRECTION('',(0.999048221581854,0.0436193873654325,-1.79912716949635E-14));
#22879=DIRECTION('center_axis',(1.09854751816067E-14,1.15185638804861E-13,
1.));
#22880=DIRECTION('ref_axis',(1.,8.73345276938534E-14,-1.09854751816168E-14));
#22881=DIRECTION('center_axis',(1.09854751816067E-14,1.15185638804861E-13,
1.));
#22882=DIRECTION('ref_axis',(1.,8.73345276938534E-14,-1.09854751816168E-14));
#22883=DIRECTION('',(0.000800685489064943,0.0174340297463221,-0.999847695156393));
#22884=DIRECTION('center_axis',(1.04854396770053E-14,1.15185638804861E-13,
1.));
#22885=DIRECTION('ref_axis',(1.,8.72905510366657E-14,-1.04854396770154E-14));
#22886=DIRECTION('',(-0.000800685489088981,0.017434029746322,-0.999847695156393));
#22887=DIRECTION('center_axis',(1.04854396770053E-14,1.15185638804861E-13,
1.));
#22888=DIRECTION('ref_axis',(1.,8.72905510366657E-14,-1.04854396770154E-14));
#22889=DIRECTION('center_axis',(1.09854751816067E-14,1.15185638804861E-13,
1.));
#22890=DIRECTION('ref_axis',(1.,8.73345276938534E-14,-1.09854751816168E-14));
#22891=DIRECTION('center_axis',(1.09854751816067E-14,1.15185638804861E-13,
1.));
#22892=DIRECTION('ref_axis',(1.,8.73345276938534E-14,-1.09854751816168E-14));
#22893=DIRECTION('center_axis',(-0.0436127439212822,-0.998896061698718,
-0.017452406437168));
#22894=DIRECTION('ref_axis',(-0.999048221581861,0.0436193873652532,-5.02437150627773E-15));
#22895=DIRECTION('',(-0.00691046665282191,0.0177702355174846,-0.999818215567357));
#22896=DIRECTION('',(0.999048221581861,-0.0436193873652517,-7.94261769905107E-15));
#22897=DIRECTION('center_axis',(0.706999085398879,-0.706999085398772,-0.0174524064372095));
#22898=DIRECTION('ref_axis',(-0.707106781186493,-0.707106781186602,8.14494986888246E-14));
#22899=DIRECTION('',(-0.0177702355176088,0.00691046665269189,-0.999818215567355));
#22900=DIRECTION('',(0.707106781186494,0.707106781186601,-9.02134649096816E-14));
#22901=DIRECTION('center_axis',(0.998896061698708,0.0436127439214494,-0.017452406437299));
#22902=DIRECTION('ref_axis',(0.0436193873654224,-0.999048221581854,1.15076006713017E-13));
#22903=DIRECTION('',(-0.0436193873654263,0.999048221581854,-1.15076007599766E-13));
#22904=DIRECTION('center_axis',(1.20840226997713E-14,1.16284186323023E-13,
1.));
#22905=DIRECTION('ref_axis',(1.,8.73345276938747E-14,-1.20840226997814E-14));
#22906=DIRECTION('center_axis',(1.20840226997713E-14,1.16284186323023E-13,
1.));
#22907=DIRECTION('ref_axis',(1.,8.73345276938747E-14,-1.20840226997814E-14));
#22908=DIRECTION('center_axis',(9.88692766344536E-15,1.12988543768537E-13,
1.));
#22909=DIRECTION('ref_axis',(1.,8.71972092540841E-14,-9.88692766345521E-15));
#22910=DIRECTION('center_axis',(9.88692766344536E-15,1.12988543768537E-13,
1.));
#22911=DIRECTION('ref_axis',(1.,8.71972092540841E-14,-9.88692766345521E-15));
#22912=DIRECTION('center_axis',(0.99888282418075,-0.0439169962041995,-0.0174470914793711));
#22913=DIRECTION('ref_axis',(-0.0439236819193947,-0.999034889364052,1.15074518868834E-13));
#22914=DIRECTION('',(-0.0177673819895374,-0.00691332094576837,-0.999818246548211));
#22915=DIRECTION('',(0.043923681919403,0.999034889364052,-1.1507447191974E-13));
#22916=DIRECTION('center_axis',(0.706999085398756,0.706999085398891,-0.0174524064373725));
#22917=DIRECTION('ref_axis',(0.707106781186616,-0.707106781186479,8.14482412682667E-14));
#22918=DIRECTION('',(-0.00691046665282119,-0.0177702355177138,-0.999818215567353));
#22919=DIRECTION('',(-0.707106781186614,0.707106781186481,-7.26836276787585E-14));
#22920=DIRECTION('center_axis',(-0.043612743921454,0.998896061698706,-0.0174524064373982));
#22921=DIRECTION('ref_axis',(0.999048221581854,0.043619387365425,-5.02429633897994E-15));
#22922=DIRECTION('',(-0.999048221581854,-0.0436193873654181,1.37629650946532E-14));
#22923=DIRECTION('center_axis',(1.03092138003367E-14,1.135996059125E-13,
1.));
#22924=DIRECTION('ref_axis',(1.,8.7231809079856E-14,-1.03092138003466E-14));
#22925=DIRECTION('center_axis',(1.03092138003367E-14,1.135996059125E-13,
1.));
#22926=DIRECTION('ref_axis',(1.,8.7231809079856E-14,-1.03092138003466E-14));
#22927=DIRECTION('',(-0.00411922378064456,-0.0169593185565058,-0.999847695156389));
#22928=DIRECTION('center_axis',(1.06396373193144E-14,1.15185638804861E-13,
1.));
#22929=DIRECTION('ref_axis',(1.,8.7275865546922E-14,-1.06396373193244E-14));
#22930=DIRECTION('',(0.00411922378062659,-0.0169593185565051,-0.999847695156389));
#22931=DIRECTION('center_axis',(1.06396373193144E-14,1.15185638804861E-13,
1.));
#22932=DIRECTION('ref_axis',(1.,8.7275865546922E-14,-1.06396373193244E-14));
#22933=DIRECTION('center_axis',(1.03092138003362E-14,1.18357704589583E-13,
1.));
#22934=DIRECTION('ref_axis',(1.,8.72318090798554E-14,-1.03092138003465E-14));
#22935=DIRECTION('center_axis',(1.03092138003362E-14,1.18357704589583E-13,
1.));
#22936=DIRECTION('ref_axis',(1.,8.72318090798554E-14,-1.03092138003465E-14));
#22937=DIRECTION('center_axis',(0.0436127439212838,0.998896061698714,-0.0174524064373991));
#22938=DIRECTION('ref_axis',(0.999048221581861,-0.0436193873652548,5.0243115308101E-15));
#22939=DIRECTION('',(0.00691046665280434,-0.0177702355177117,-0.999818215567353));
#22940=DIRECTION('',(-0.999048221581863,0.0436193873652139,3.71431109875224E-15));
#22941=DIRECTION('center_axis',(-0.706999085398881,0.706999085398766,-0.0174524064373575));
#22942=DIRECTION('ref_axis',(0.707106781186491,0.707106781186604,-8.14480637193561E-14));
#22943=DIRECTION('',(0.0177702355175879,-0.00691046665292151,-0.999818215567354));
#22944=DIRECTION('',(-0.707106781186494,-0.707106781186601,9.02134649096816E-14));
#22945=DIRECTION('center_axis',(-0.998896061698709,-0.0436127439214501,
-0.0174524064372681));
#22946=DIRECTION('ref_axis',(-0.0436193873654191,0.999048221581854,-1.15076106866482E-13));
#22947=DIRECTION('',(0.0436193873654296,-0.999048221581854,1.15076007599765E-13));
#22948=DIRECTION('center_axis',(1.09854751816069E-14,1.14087091286699E-13,
1.));
#22949=DIRECTION('ref_axis',(1.,8.71972092540835E-14,-1.09854751816168E-14));
#22950=DIRECTION('center_axis',(1.09854751816069E-14,1.14087091286699E-13,
1.));
#22951=DIRECTION('ref_axis',(1.,8.71972092540835E-14,-1.09854751816168E-14));
#22952=DIRECTION('',(0.0174340297464268,-0.000800685489190584,-0.999847695156391));
#22953=DIRECTION('center_axis',(1.04854396770055E-14,1.1301218632279E-13,
1.));
#22954=DIRECTION('ref_axis',(-1.,-8.71405510634815E-14,1.04854396770154E-14));
#22955=DIRECTION('center_axis',(1.04854396770055E-14,1.1301218632279E-13,
1.));
#22956=DIRECTION('ref_axis',(1.,8.72630157433963E-14,-1.04854396770154E-14));
#22957=DIRECTION('center_axis',(-1.00515054169548E-26,1.1518563880486E-13,
1.));
#22958=DIRECTION('ref_axis',(-8.72635297355373E-14,1.,-1.1518563880486E-13));
#22959=DIRECTION('',(8.72635297355373E-14,-1.,1.1518563880486E-13));
#22960=DIRECTION('',(-8.72635297355373E-14,1.,-1.1518563880486E-13));
#22961=DIRECTION('',(-1.,-8.72635297355373E-14,0.));
#22962=DIRECTION('center_axis',(-0.866025403795548,-1.79796141756299E-14,
0.499999999980758));
#22963=DIRECTION('ref_axis',(0.499999999980758,1.43385454223517E-13,0.866025403795548));
#22964=DIRECTION('',(-8.72635297355373E-14,1.,-1.1518563880486E-13));
#22965=DIRECTION('',(-0.499999999980757,-1.43385454223517E-13,-0.866025403795548));
#22966=DIRECTION('center_axis',(-0.866025403795548,-1.33165252976057E-13,
-0.499999999980758));
#22967=DIRECTION('ref_axis',(-0.499999999980758,5.61219244913375E-14,0.866025403795548));
#22968=DIRECTION('',(-8.72635297355373E-14,1.,-1.1518563880486E-13));
#22969=DIRECTION('',(0.499999999980757,-5.61219244913376E-14,-0.866025403795548));
#22970=DIRECTION('center_axis',(1.00515054169548E-26,-1.1518563880486E-13,
-1.));
#22971=DIRECTION('ref_axis',(8.72635297355373E-14,-1.,1.1518563880486E-13));
#22972=DIRECTION('',(-8.72635297355373E-14,1.,-1.1518563880486E-13));
#22973=DIRECTION('',(1.,8.72635297355373E-14,0.));
#22974=DIRECTION('center_axis',(0.866025403795548,1.79796141756299E-14,
-0.499999999980758));
#22975=DIRECTION('ref_axis',(-0.499999999980758,-1.43385454223517E-13,-0.866025403795548));
#22976=DIRECTION('',(-8.72635297355373E-14,1.,-1.1518563880486E-13));
#22977=DIRECTION('',(0.499999999980757,1.43385454223517E-13,0.866025403795548));
#22978=DIRECTION('center_axis',(0.866025403795548,1.33165252976057E-13,
0.499999999980758));
#22979=DIRECTION('ref_axis',(0.499999999980758,-5.61219244913375E-14,-0.866025403795548));
#22980=DIRECTION('',(-0.499999999980757,5.61219244913376E-14,0.866025403795548));
#22981=DIRECTION('center_axis',(-1.00515054169548E-26,1.1518563880486E-13,
1.));
#22982=DIRECTION('ref_axis',(-8.72635297355373E-14,1.,-1.1518563880486E-13));
#22983=DIRECTION('',(8.72635297355373E-14,-1.,1.1518563880486E-13));
#22984=DIRECTION('',(-8.72635297355373E-14,1.,-1.1518563880486E-13));
#22985=DIRECTION('',(-1.,-8.72635297355373E-14,0.));
#22986=DIRECTION('center_axis',(-0.866025403795548,-1.79796141756299E-14,
0.499999999980758));
#22987=DIRECTION('ref_axis',(0.499999999980758,1.43385454223517E-13,0.866025403795548));
#22988=DIRECTION('',(-8.72635297355373E-14,1.,-1.1518563880486E-13));
#22989=DIRECTION('',(-0.499999999980758,-1.43385454223516E-13,-0.866025403795548));
#22990=DIRECTION('center_axis',(-0.866025403795548,-1.33165252976057E-13,
-0.499999999980758));
#22991=DIRECTION('ref_axis',(-0.499999999980758,5.61219244913375E-14,0.866025403795548));
#22992=DIRECTION('',(-8.72635297355373E-14,1.,-1.1518563880486E-13));
#22993=DIRECTION('',(0.499999999980758,-5.61219244913375E-14,-0.866025403795548));
#22994=DIRECTION('center_axis',(1.00515054169548E-26,-1.1518563880486E-13,
-1.));
#22995=DIRECTION('ref_axis',(8.72635297355373E-14,-1.,1.1518563880486E-13));
#22996=DIRECTION('',(-8.72635297355373E-14,1.,-1.1518563880486E-13));
#22997=DIRECTION('',(1.,8.72635297355373E-14,0.));
#22998=DIRECTION('center_axis',(0.866025403795548,1.79796141756299E-14,
-0.499999999980758));
#22999=DIRECTION('ref_axis',(-0.499999999980758,-1.43385454223517E-13,-0.866025403795548));
#23000=DIRECTION('',(-8.72635297355373E-14,1.,-1.1518563880486E-13));
#23001=DIRECTION('',(0.499999999980757,1.43385454223517E-13,0.866025403795548));
#23002=DIRECTION('center_axis',(0.866025403795548,1.33165252976057E-13,
0.499999999980758));
#23003=DIRECTION('ref_axis',(0.499999999980758,-5.61219244913375E-14,-0.866025403795548));
#23004=DIRECTION('',(-0.499999999980757,5.61219244913376E-14,0.866025403795548));
#23005=DIRECTION('center_axis',(1.00515054169548E-26,-1.1518563880486E-13,
-1.));
#23006=DIRECTION('ref_axis',(8.72635297355373E-14,-1.,1.1518563880486E-13));
#23007=DIRECTION('center_axis',(1.00515054169548E-26,-1.1518563880486E-13,
-1.));
#23008=DIRECTION('ref_axis',(8.72635297355373E-14,-1.,1.1518563880486E-13));
#23009=DIRECTION('',(1.00515054169548E-26,-1.1518563880486E-13,-1.));
#23010=DIRECTION('center_axis',(1.00515054169548E-26,-1.1518563880486E-13,
-1.));
#23011=DIRECTION('ref_axis',(8.72635297355373E-14,-1.,1.1518563880486E-13));
#23012=DIRECTION('',(-1.00515054169548E-26,1.1518563880486E-13,1.));
#23013=DIRECTION('center_axis',(1.00515054169548E-26,-1.1518563880486E-13,
-1.));
#23014=DIRECTION('ref_axis',(8.72635297355373E-14,-1.,1.1518563880486E-13));
#23015=DIRECTION('center_axis',(1.00515054169548E-26,-1.1518563880486E-13,
-1.));
#23016=DIRECTION('ref_axis',(8.72635297355373E-14,-1.,1.1518563880486E-13));
#23017=DIRECTION('',(-1.00515054169548E-26,1.1518563880486E-13,1.));
#23018=DIRECTION('center_axis',(1.00515054169548E-26,-1.1518563880486E-13,
-1.));
#23019=DIRECTION('ref_axis',(8.72635297355373E-14,-1.,1.1518563880486E-13));
#23020=DIRECTION('',(1.00515054169548E-26,-1.1518563880486E-13,-1.));
#23021=DIRECTION('center_axis',(-8.72635297355373E-14,1.,-1.1518563880486E-13));
#23022=DIRECTION('ref_axis',(1.00515054169548E-26,-1.1518563880486E-13,
-1.));
#23023=DIRECTION('',(1.00515054169548E-26,-1.1518563880486E-13,-1.));
#23024=DIRECTION('',(-1.,-8.72635297355373E-14,0.));
#23025=DIRECTION('',(-8.97974505221575E-16,1.1518563880486E-13,1.));
#23026=DIRECTION('',(1.,8.72635297355374E-14,6.53072367426562E-16));
#23027=DIRECTION('center_axis',(-1.00515054169548E-26,1.1518563880486E-13,
1.));
#23028=DIRECTION('ref_axis',(-8.72635297355373E-14,1.,-1.1518563880486E-13));
#23029=DIRECTION('',(0.997564050259831,-0.0697564737440288,8.03494398899043E-15));
#23030=DIRECTION('center_axis',(1.00515054169548E-26,-1.1518563880486E-13,
-1.));
#23031=DIRECTION('ref_axis',(8.72635297355373E-14,-1.,1.1518563880486E-13));
#23032=DIRECTION('',(0.997564050259819,0.069756473744203,-8.03494398899043E-15));
#23033=DIRECTION('',(-8.72635297355373E-14,1.,-1.1518563880486E-13));
#23034=DIRECTION('',(8.72635297355373E-14,-1.,1.1518563880486E-13));
#23035=DIRECTION('center_axis',(1.00515054169548E-26,-1.1518563880486E-13,
-1.));
#23036=DIRECTION('ref_axis',(-8.7385994415452E-14,1.,-1.1518563880486E-13));
#23037=DIRECTION('',(1.00515054169548E-26,-1.1518563880486E-13,-1.));
#23038=DIRECTION('',(-1.00515054169548E-26,1.1518563880486E-13,1.));
#23039=DIRECTION('center_axis',(1.00515054169548E-26,-1.1518563880486E-13,
-1.));
#23040=DIRECTION('ref_axis',(8.72635297355373E-14,-1.,1.1518563880486E-13));
#23041=DIRECTION('center_axis',(1.00515054169548E-26,-1.1518563880486E-13,
-1.));
#23042=DIRECTION('ref_axis',(8.72635297355373E-14,-1.,1.1518563880486E-13));
#23043=DIRECTION('center_axis',(1.00515054169548E-26,-1.1518563880486E-13,
-1.));
#23044=DIRECTION('ref_axis',(8.72635297355373E-14,-1.,1.1518563880486E-13));
#23045=DIRECTION('',(-1.00515054169548E-26,1.1518563880486E-13,1.));
#23046=DIRECTION('center_axis',(1.00515054169548E-26,-1.1518563880486E-13,
-1.));
#23047=DIRECTION('ref_axis',(8.72635297355373E-14,-1.,1.1518563880486E-13));
#23048=DIRECTION('',(1.00515054169548E-26,-1.1518563880486E-13,-1.));
#23049=DIRECTION('center_axis',(1.00515054169548E-26,-1.1518563880486E-13,
-1.));
#23050=DIRECTION('ref_axis',(8.72635297355373E-14,-1.,1.1518563880486E-13));
#23051=DIRECTION('center_axis',(1.00515054169548E-26,-1.1518563880486E-13,
-1.));
#23052=DIRECTION('ref_axis',(8.72635297355373E-14,-1.,1.1518563880486E-13));
#23053=DIRECTION('',(1.00515054169548E-26,-1.1518563880486E-13,-1.));
#23054=DIRECTION('center_axis',(1.00515054169548E-26,-1.1518563880486E-13,
-1.));
#23055=DIRECTION('ref_axis',(8.72635297355373E-14,-1.,1.1518563880486E-13));
#23056=DIRECTION('',(-1.00515054169548E-26,1.1518563880486E-13,1.));
#23057=DIRECTION('center_axis',(1.00515054169548E-26,-1.1518563880486E-13,
-1.));
#23058=DIRECTION('ref_axis',(8.72635297355373E-14,-1.,1.1518563880486E-13));
#23059=DIRECTION('center_axis',(1.00515054169548E-26,-1.1518563880486E-13,
-1.));
#23060=DIRECTION('ref_axis',(8.72635297355373E-14,-1.,1.1518563880486E-13));
#23061=DIRECTION('',(-1.00515054169548E-26,1.1518563880486E-13,1.));
#23062=DIRECTION('center_axis',(1.00515054169548E-26,-1.1518563880486E-13,
-1.));
#23063=DIRECTION('ref_axis',(8.72635297355373E-14,-1.,1.1518563880486E-13));
#23064=DIRECTION('',(1.00515054169548E-26,-1.1518563880486E-13,-1.));
#23065=DIRECTION('center_axis',(1.04744440165193E-14,1.15185638804861E-13,
1.));
#23066=DIRECTION('ref_axis',(1.,8.72635297355361E-14,-1.04744440165294E-14));
#23067=DIRECTION('',(0.0697564737442121,-0.997564050259818,1.14905052377941E-13));
#23068=DIRECTION('',(-0.0697564737440384,-0.99756405025983,1.14905052377941E-13));
#23069=DIRECTION('',(-0.997564050259819,-0.069756473744203,8.03494398899043E-15));
#23070=DIRECTION('',(-0.997564050259831,0.0697564737440288,-8.03494398899043E-15));
#23071=DIRECTION('',(-0.069756473744214,0.997564050259818,-1.14905052377941E-13));
#23072=DIRECTION('',(0.0697564737440366,0.997564050259831,-1.14905052377941E-13));
#23073=DIRECTION('center_axis',(-1.00515054169548E-26,1.1518563880486E-13,
1.));
#23074=DIRECTION('ref_axis',(8.72635297355373E-14,-1.,1.1518563880486E-13));
#23075=DIRECTION('',(0.997564050259819,0.0697564737442016,-8.03494398899027E-15));
#23076=DIRECTION('',(0.997564050259831,-0.0697564737440285,8.03494398899039E-15));
#23077=DIRECTION('center_axis',(1.00515054169548E-26,-1.1518563880486E-13,
-1.));
#23078=DIRECTION('ref_axis',(8.72635297355373E-14,-1.,1.1518563880486E-13));
#23079=DIRECTION('center_axis',(1.00515054169548E-26,-1.1518563880486E-13,
-1.));
#23080=DIRECTION('ref_axis',(8.72635297355373E-14,-1.,1.1518563880486E-13));
#23081=DIRECTION('',(-1.00515054169548E-26,1.1518563880486E-13,1.));
#23082=DIRECTION('',(1.00515054169548E-26,-1.1518563880486E-13,-1.));
#23083=DIRECTION('center_axis',(-8.72635297355373E-14,1.,-1.1518563880486E-13));
#23084=DIRECTION('ref_axis',(1.00515054169548E-26,-1.1518563880486E-13,
-1.));
#23085=DIRECTION('center_axis',(-8.72635297355373E-14,1.,-1.1518563880486E-13));
#23086=DIRECTION('ref_axis',(1.00515054169548E-26,-1.1518563880486E-13,
-1.));
#23087=DIRECTION('center_axis',(0.997564050259831,-0.0697564737440366,8.03494398899132E-15));
#23088=DIRECTION('ref_axis',(-0.0697564737440366,-0.997564050259831,1.14905052377941E-13));
#23089=DIRECTION('',(-0.0697564737440395,-0.99756405025983,1.14905052377941E-13));
#23090=DIRECTION('',(-1.00515054169548E-26,1.1518563880486E-13,1.));
#23091=DIRECTION('',(-0.069756473744048,-0.99756405025983,1.14905052377941E-13));
#23092=DIRECTION('center_axis',(0.997564050259818,0.069756473744214,-8.0349439889917E-15));
#23093=DIRECTION('ref_axis',(0.069756473744214,-0.997564050259818,1.14905052377941E-13));
#23094=DIRECTION('',(0.0697564737442205,-0.997564050259818,1.14905052377941E-13));
#23095=DIRECTION('',(1.00515054169548E-26,-1.1518563880486E-13,-1.));
#23096=DIRECTION('',(0.069756473744213,-0.997564050259818,1.14905052377941E-13));
#23097=DIRECTION('center_axis',(-1.00515054169548E-26,1.1518563880486E-13,
1.));
#23098=DIRECTION('ref_axis',(-8.72635297355373E-14,1.,-1.1518563880486E-13));
#23099=DIRECTION('',(1.,8.67672446588636E-14,5.71649135859831E-29));
#23100=DIRECTION('center_axis',(-1.00515054169548E-26,1.1518563880486E-13,
1.));
#23101=DIRECTION('ref_axis',(-8.67361737988403E-14,1.,-1.1518563880486E-13));
#23102=DIRECTION('',(0.374606593415996,-0.927183854566754,1.06798264577828E-13));
#23103=DIRECTION('',(8.72635297355373E-14,-1.,1.1518563880486E-13));
#23104=DIRECTION('',(-0.374606593415834,-0.927183854566819,1.06798264577828E-13));
#23105=DIRECTION('center_axis',(-1.00515054169548E-26,1.1518563880486E-13,
1.));
#23106=DIRECTION('ref_axis',(-8.67361737988403E-14,1.,-1.1518563880486E-13));
#23107=DIRECTION('',(-1.,-8.7759814812211E-14,5.71649135859831E-29));
#23108=DIRECTION('center_axis',(-1.00515054169548E-26,1.1518563880486E-13,
1.));
#23109=DIRECTION('ref_axis',(-8.74300631892311E-14,1.,-1.1518563880486E-13));
#23110=DIRECTION('',(-1.00515054169548E-26,1.1518563880486E-13,1.));
#23111=DIRECTION('center_axis',(1.00515054169548E-26,-1.1518563880486E-13,
-1.));
#23112=DIRECTION('ref_axis',(-8.60422844084497E-14,1.,-1.1518563880486E-13));
#23113=DIRECTION('',(1.00515054169548E-26,-1.1518563880486E-13,-1.));
#23114=DIRECTION('center_axis',(1.00515054169548E-26,-1.1518563880486E-13,
-1.));
#23115=DIRECTION('ref_axis',(-8.88178419700126E-14,1.,-1.1518563880486E-13));
#23116=DIRECTION('center_axis',(0.0697564737440288,0.997564050259831,-1.14905052377941E-13));
#23117=DIRECTION('ref_axis',(0.997564050259831,-0.0697564737440288,8.03494398899043E-15));
#23118=DIRECTION('',(-1.00515054169548E-26,1.1518563880486E-13,1.));
#23119=DIRECTION('',(0.997564050259829,-0.0697564737440514,8.03494398899303E-15));
#23120=DIRECTION('',(-1.00515054169548E-26,1.1518563880486E-13,1.));
#23121=DIRECTION('',(0.997564050259831,-0.0697564737440331,8.03494398899092E-15));
#23122=DIRECTION('center_axis',(1.00515054169548E-26,-1.1518563880486E-13,
-1.));
#23123=DIRECTION('ref_axis',(8.72635297355373E-14,-1.,1.1518563880486E-13));
#23124=DIRECTION('',(8.67672446588636E-14,-1.,1.1518563880486E-13));
#23125=DIRECTION('',(1.,8.67672446588636E-14,5.71649135859831E-29));
#23126=DIRECTION('center_axis',(-1.00515054169548E-26,1.1518563880486E-13,
1.));
#23127=DIRECTION('ref_axis',(-8.72635297355373E-14,1.,-1.1518563880486E-13));
#23128=DIRECTION('',(-0.927183854566823,0.374606593415825,-4.31492997631236E-14));
#23129=DIRECTION('center_axis',(-1.00515054169548E-26,1.1518563880486E-13,
1.));
#23130=DIRECTION('ref_axis',(-8.67361737988404E-14,1.,-1.1518563880486E-13));
#23131=DIRECTION('',(8.67672446588636E-14,-1.,1.1518563880486E-13));
#23132=DIRECTION('',(-8.72635297355373E-14,1.,-1.1518563880486E-13));
#23133=DIRECTION('center_axis',(-1.,-8.72635297355373E-14,0.));
#23134=DIRECTION('ref_axis',(-8.72635297355373E-14,1.,-1.1518563880486E-13));
#23135=DIRECTION('',(1.00515054169548E-26,-1.1518563880486E-13,-1.));
#23136=DIRECTION('',(8.72635297355373E-14,-1.,1.1518563880486E-13));
#23137=DIRECTION('center_axis',(1.,8.72635297355374E-14,8.97974505211524E-16));
#23138=DIRECTION('ref_axis',(8.97974505221575E-16,-1.1518563880486E-13,
-1.));
#23139=DIRECTION('',(-1.00515054169548E-26,1.1518563880486E-13,1.));
#23140=DIRECTION('',(-8.72635297355373E-14,1.,-1.1518563880486E-13));
#23141=DIRECTION('',(1.00515054169548E-26,-1.1518563880486E-13,-1.));
#23142=DIRECTION('',(-8.72635297355373E-14,1.,-1.1518563880486E-13));
#23143=DIRECTION('center_axis',(6.53072367436613E-16,-1.1518563880486E-13,
-1.));
#23144=DIRECTION('ref_axis',(-1.,-8.72635297355374E-14,-6.53072367426562E-16));
#23145=DIRECTION('',(0.927183854566753,0.374606593415997,-4.31492997631248E-14));
#23146=DIRECTION('',(1.,8.72635297355373E-14,0.));
#23147=DIRECTION('',(0.927183854566819,-0.374606593415835,4.31492997631247E-14));
#23148=DIRECTION('center_axis',(-0.069756473744203,0.997564050259819,-1.14905052377941E-13));
#23149=DIRECTION('ref_axis',(0.997564050259819,0.069756473744203,-8.03494398899043E-15));
#23150=DIRECTION('',(1.00515054169548E-26,-1.1518563880486E-13,-1.));
#23151=DIRECTION('',(0.997564050259817,0.0697564737442254,-8.03494398899302E-15));
#23152=DIRECTION('',(0.997564050259819,0.0697564737442072,-8.03494398899092E-15));
#23153=DIRECTION('center_axis',(-1.00515054169548E-26,1.1518563880486E-13,
1.));
#23154=DIRECTION('ref_axis',(-8.72635297355373E-14,1.,-1.1518563880486E-13));
#23155=DIRECTION('',(-8.7759814812211E-14,1.,-1.1518563880486E-13));
#23156=DIRECTION('center_axis',(-1.00515054169548E-26,1.1518563880486E-13,
1.));
#23157=DIRECTION('ref_axis',(-8.67361737988404E-14,1.,-1.1518563880486E-13));
#23158=DIRECTION('',(0.927183854566753,0.374606593415997,-4.31492997631248E-14));
#23159=DIRECTION('center_axis',(-1.00515054169548E-26,1.1518563880486E-13,
1.));
#23160=DIRECTION('ref_axis',(-8.74300631892311E-14,1.,-1.1518563880486E-13));
#23161=DIRECTION('',(-1.00515054169548E-26,1.1518563880486E-13,1.));
#23162=DIRECTION('center_axis',(1.00515054169548E-26,-1.1518563880486E-13,
-1.));
#23163=DIRECTION('ref_axis',(-8.74300631892311E-14,1.,-1.1518563880486E-13));
#23164=DIRECTION('',(1.00515054169548E-26,-1.1518563880486E-13,-1.));
#23165=DIRECTION('center_axis',(1.00515054169548E-26,-1.1518563880486E-13,
-1.));
#23166=DIRECTION('ref_axis',(-8.74300631892311E-14,1.,-1.1518563880486E-13));
#23167=DIRECTION('center_axis',(-0.99756405025983,0.0697564737440384,-8.03494398899153E-15));
#23168=DIRECTION('ref_axis',(0.0697564737440384,0.99756405025983,-1.14905052377941E-13));
#23169=DIRECTION('',(0.0697564737440399,0.99756405025983,-1.14905052377941E-13));
#23170=DIRECTION('',(-1.00515054169548E-26,1.1518563880486E-13,1.));
#23171=DIRECTION('',(0.069756473744023,0.997564050259831,-1.14905052377941E-13));
#23172=DIRECTION('center_axis',(1.00515054169548E-26,-1.1518563880486E-13,
-1.));
#23173=DIRECTION('ref_axis',(8.72635297355373E-14,-1.,1.1518563880486E-13));
#23174=DIRECTION('',(1.,8.7759814812211E-14,-5.71649135859831E-29));
#23175=DIRECTION('',(-8.7759814812211E-14,1.,-1.1518563880486E-13));
#23176=DIRECTION('center_axis',(-0.997564050259818,-0.0697564737442121,
8.03494398899149E-15));
#23177=DIRECTION('ref_axis',(-0.0697564737442121,0.997564050259818,-1.14905052377941E-13));
#23178=DIRECTION('',(-0.069756473744197,0.997564050259819,-1.14905052377941E-13));
#23179=DIRECTION('',(1.00515054169548E-26,-1.1518563880486E-13,-1.));
#23180=DIRECTION('',(-0.0697564737442141,0.997564050259818,-1.14905052377941E-13));
#23181=DIRECTION('center_axis',(-1.00515054169548E-26,1.1518563880486E-13,
1.));
#23182=DIRECTION('ref_axis',(-8.72635297355373E-14,1.,-1.1518563880486E-13));
#23183=DIRECTION('',(-1.,-8.67672446588636E-14,-5.71649135859831E-29));
#23184=DIRECTION('center_axis',(-1.00515054169548E-26,1.1518563880486E-13,
1.));
#23185=DIRECTION('ref_axis',(-8.67361737988403E-14,1.,-1.1518563880486E-13));
#23186=DIRECTION('',(-0.374606593415996,0.927183854566754,-1.06798264577828E-13));
#23187=DIRECTION('',(-8.72635297355373E-14,1.,-1.1518563880486E-13));
#23188=DIRECTION('',(0.374606593415834,0.927183854566819,-1.06798264577828E-13));
#23189=DIRECTION('center_axis',(-1.00515054169548E-26,1.1518563880486E-13,
1.));
#23190=DIRECTION('ref_axis',(-8.67361737988404E-14,1.,-1.1518563880486E-13));
#23191=DIRECTION('',(1.,8.7759814812211E-14,-5.71649135859831E-29));
#23192=DIRECTION('center_axis',(-1.00515054169548E-26,1.1518563880486E-13,
1.));
#23193=DIRECTION('ref_axis',(-8.74300631892311E-14,1.,-1.1518563880486E-13));
#23194=DIRECTION('',(-1.00515054169548E-26,1.1518563880486E-13,1.));
#23195=DIRECTION('center_axis',(1.00515054169548E-26,-1.1518563880486E-13,
-1.));
#23196=DIRECTION('ref_axis',(-8.04911692853239E-14,1.,-1.1518563880486E-13));
#23197=DIRECTION('',(1.00515054169548E-26,-1.1518563880486E-13,-1.));
#23198=DIRECTION('center_axis',(1.00515054169548E-26,-1.1518563880486E-13,
-1.));
#23199=DIRECTION('ref_axis',(-8.04911692853239E-14,1.,-1.1518563880486E-13));
#23200=DIRECTION('center_axis',(-0.0697564737440285,-0.997564050259831,
1.14905052377941E-13));
#23201=DIRECTION('ref_axis',(-0.997564050259831,0.0697564737440285,-8.03494398899039E-15));
#23202=DIRECTION('',(-0.997564050259831,0.0697564737440297,-8.03494398899053E-15));
#23203=DIRECTION('',(-1.00515054169548E-26,1.1518563880486E-13,1.));
#23204=DIRECTION('',(-0.997564050259831,0.0697564737440314,-8.03494398899072E-15));
#23205=DIRECTION('center_axis',(1.00515054169548E-26,-1.1518563880486E-13,
-1.));
#23206=DIRECTION('ref_axis',(8.72635297355373E-14,-1.,1.1518563880486E-13));
#23207=DIRECTION('',(-8.67672446588636E-14,1.,-1.1518563880486E-13));
#23208=DIRECTION('',(-1.,-8.67672446588636E-14,-5.71649135859831E-29));
#23209=DIRECTION('center_axis',(-1.00515054169548E-26,1.1518563880486E-13,
1.));
#23210=DIRECTION('ref_axis',(-8.74300631892311E-14,1.,-1.1518563880486E-13));
#23211=DIRECTION('',(-1.00515054169548E-26,1.1518563880486E-13,1.));
#23212=DIRECTION('center_axis',(1.00515054169548E-26,-1.1518563880486E-13,
-1.));
#23213=DIRECTION('ref_axis',(-1.13797860024079E-13,1.,-1.1518563880486E-13));
#23214=DIRECTION('',(1.00515054169548E-26,-1.1518563880486E-13,-1.));
#23215=DIRECTION('center_axis',(1.00515054169548E-26,-1.1518563880486E-13,
-1.));
#23216=DIRECTION('ref_axis',(-1.13797860024079E-13,1.,-1.1518563880486E-13));
#23217=DIRECTION('center_axis',(1.00515054169548E-26,-1.1518563880486E-13,
-1.));
#23218=DIRECTION('ref_axis',(8.72635297355373E-14,-1.,1.1518563880486E-13));
#23219=DIRECTION('',(-1.,-8.7759814812211E-14,5.71649135859831E-29));
#23220=DIRECTION('',(8.7759814812211E-14,-1.,1.1518563880486E-13));
#23221=DIRECTION('',(-0.997564050259819,-0.0697564737442016,8.03494398899027E-15));
#23222=DIRECTION('center_axis',(0.0697564737442016,-0.997564050259819,1.14905052377941E-13));
#23223=DIRECTION('ref_axis',(-0.997564050259819,-0.0697564737442016,8.03494398899027E-15));
#23224=DIRECTION('',(1.00515054169548E-26,-1.1518563880486E-13,-1.));
#23225=DIRECTION('',(-0.997564050259819,-0.0697564737441972,8.03494398898977E-15));
#23226=DIRECTION('center_axis',(-1.00515054169548E-26,1.1518563880486E-13,
1.));
#23227=DIRECTION('ref_axis',(-8.72635297355373E-14,1.,-1.1518563880486E-13));
#23228=DIRECTION('',(8.7759814812211E-14,-1.,1.1518563880486E-13));
#23229=DIRECTION('center_axis',(-1.00515054169548E-26,1.1518563880486E-13,
1.));
#23230=DIRECTION('ref_axis',(-8.67361737988403E-14,1.,-1.1518563880486E-13));
#23231=DIRECTION('',(-0.927183854566753,-0.374606593415997,4.31492997631248E-14));
#23232=DIRECTION('',(-1.,-8.72635297355373E-14,0.));
#23233=DIRECTION('',(-0.927183854566819,0.374606593415835,-4.31492997631247E-14));
#23234=DIRECTION('center_axis',(-1.00515054169548E-26,1.1518563880486E-13,
1.));
#23235=DIRECTION('ref_axis',(-8.67361737988403E-14,1.,-1.1518563880486E-13));
#23236=DIRECTION('',(-8.67672446588636E-14,1.,-1.1518563880486E-13));
#23237=DIRECTION('center_axis',(0.868162779195958,0.359604797490614,0.34202014332563));
#23238=DIRECTION('ref_axis',(0.382683432365172,-0.923879532511253,1.06407127951475E-13));
#23239=DIRECTION('',(0.145459785961516,0.474519896165923,-0.868143029005423));
#23240=DIRECTION('',(0.483645502898238,-0.458543714227443,-0.745536511291574));
#23241=DIRECTION('',(0.338019145174967,-0.933063205484026,0.123028907444791));
#23242=DIRECTION('',(-0.145459785961518,-0.474519896165925,0.868143029005422));
#23243=DIRECTION('',(-0.483645502898236,0.458543714227446,0.745536511291574));
#23244=DIRECTION('',(-0.338019145174969,0.933063205484025,-0.123028907444792));
#23245=DIRECTION('center_axis',(8.72635297355373E-14,-1.,1.1518563880486E-13));
#23246=DIRECTION('ref_axis',(-1.00515054169548E-26,1.1518563880486E-13,
1.));
#23247=DIRECTION('',(-1.,-8.72635297355373E-14,0.));
#23248=DIRECTION('',(-1.00515054169548E-26,1.1518563880486E-13,1.));
#23249=DIRECTION('',(-1.,-8.72635297355373E-14,0.));
#23250=DIRECTION('',(1.00515054169548E-26,-1.1518563880486E-13,-1.));
#23251=DIRECTION('center_axis',(-1.00515054169548E-26,1.1518563880486E-13,
1.));
#23252=DIRECTION('ref_axis',(-8.72635297355373E-14,1.,-1.1518563880486E-13));
#23253=DIRECTION('center_axis',(1.00515054169548E-26,-1.1518563880486E-13,
-1.));
#23254=DIRECTION('ref_axis',(8.72635297355373E-14,-1.,1.1518563880486E-13));
#23255=DIRECTION('',(-0.997564050259819,-0.0697564737442026,8.03494398899039E-15));
#23256=DIRECTION('',(-8.7759814812211E-14,1.,-1.1518563880486E-13));
#23257=DIRECTION('',(1.,8.7759814812211E-14,-5.71649135859831E-29));
#23258=DIRECTION('',(-0.0697564737440384,-0.99756405025983,1.14905052377941E-13));
#23259=DIRECTION('center_axis',(-1.00515054169548E-26,1.1518563880486E-13,
1.));
#23260=DIRECTION('ref_axis',(-8.72635297355373E-14,1.,-1.1518563880486E-13));
#23261=DIRECTION('center_axis',(-1.00515054169548E-26,1.1518563880486E-13,
1.));
#23262=DIRECTION('ref_axis',(-8.72635297355373E-14,1.,-1.1518563880486E-13));
#23263=DIRECTION('',(-1.00515054169548E-26,1.1518563880486E-13,1.));
#23264=DIRECTION('center_axis',(1.00515054169548E-26,-1.1518563880486E-13,
-1.));
#23265=DIRECTION('ref_axis',(-8.01581023779363E-14,1.,-1.1518563880486E-13));
#23266=DIRECTION('',(1.00515054169548E-26,-1.1518563880486E-13,-1.));
#23267=DIRECTION('center_axis',(-8.7759814812211E-14,1.,-1.1518563880486E-13));
#23268=DIRECTION('ref_axis',(1.,8.7759814812211E-14,-5.71649135859828E-29));
#23269=DIRECTION('',(1.00515054169548E-26,-1.1518563880486E-13,-1.));
#23270=DIRECTION('',(1.,8.72635297355373E-14,0.));
#23271=DIRECTION('',(1.00515054169548E-26,-1.1518563880486E-13,-1.));
#23272=DIRECTION('center_axis',(-1.00515054169548E-26,1.1518563880486E-13,
1.));
#23273=DIRECTION('ref_axis',(-8.67361737988403E-14,1.,-1.1518563880486E-13));
#23274=DIRECTION('',(-1.00515054169548E-26,1.1518563880486E-13,1.));
#23275=DIRECTION('center_axis',(-1.00515054169548E-26,1.1518563880486E-13,
1.));
#23276=DIRECTION('ref_axis',(-8.67361737988403E-14,1.,-1.1518563880486E-13));
#23277=DIRECTION('center_axis',(-0.927183854566819,0.374606593415834,-4.31492997631247E-14));
#23278=DIRECTION('ref_axis',(0.374606593415834,0.927183854566819,-1.06798264577828E-13));
#23279=DIRECTION('',(-1.00515054169548E-26,1.1518563880486E-13,1.));
#23280=DIRECTION('',(0.374606593415835,0.927183854566819,-1.06798264577828E-13));
#23281=DIRECTION('center_axis',(-1.,-8.72635297355373E-14,0.));
#23282=DIRECTION('ref_axis',(-8.72635297355373E-14,1.,-1.1518563880486E-13));
#23283=DIRECTION('',(-1.00515054169548E-26,1.1518563880486E-13,1.));
#23284=DIRECTION('',(-8.72635297355373E-14,1.,-1.1518563880486E-13));
#23285=DIRECTION('center_axis',(-0.927183854566754,-0.374606593415996,4.31492997631246E-14));
#23286=DIRECTION('ref_axis',(-0.374606593415996,0.927183854566754,-1.06798264577828E-13));
#23287=DIRECTION('',(1.00515054169548E-26,-1.1518563880486E-13,-1.));
#23288=DIRECTION('',(-0.374606593415997,0.927183854566753,-1.06798264577828E-13));
#23289=DIRECTION('center_axis',(-1.00515054169548E-26,1.1518563880486E-13,
1.));
#23290=DIRECTION('ref_axis',(-8.67361737988403E-14,1.,-1.1518563880486E-13));
#23291=DIRECTION('',(-1.00515054169548E-26,1.1518563880486E-13,1.));
#23292=DIRECTION('center_axis',(-1.00515054169548E-26,1.1518563880486E-13,
1.));
#23293=DIRECTION('ref_axis',(-8.67361737988404E-14,1.,-1.1518563880486E-13));
#23294=DIRECTION('center_axis',(8.67672446588636E-14,-1.,1.1518563880486E-13));
#23295=DIRECTION('ref_axis',(-1.,-8.67672446588636E-14,-5.71649135859828E-29));
#23296=DIRECTION('',(-1.,-8.72635297355373E-14,0.));
#23297=DIRECTION('',(-1.00515054169548E-26,1.1518563880486E-13,1.));
#23298=DIRECTION('',(-1.,-8.72635297355373E-14,0.));
#23299=DIRECTION('center_axis',(1.00515054169548E-26,-1.1518563880486E-13,
-1.));
#23300=DIRECTION('ref_axis',(8.72635297355373E-14,-1.,1.1518563880486E-13));
#23301=DIRECTION('',(0.0697564737442125,-0.997564050259818,1.14905052377941E-13));
#23302=DIRECTION('',(-8.67672446588636E-14,1.,-1.1518563880486E-13));
#23303=DIRECTION('',(0.997564050259831,-0.0697564737440285,8.03494398899039E-15));
#23304=DIRECTION('center_axis',(-1.00515054169548E-26,1.1518563880486E-13,
1.));
#23305=DIRECTION('ref_axis',(-8.72635297355373E-14,1.,-1.1518563880486E-13));
#23306=DIRECTION('center_axis',(-1.00515054169548E-26,1.1518563880486E-13,
1.));
#23307=DIRECTION('ref_axis',(-8.72635297355373E-14,1.,-1.1518563880486E-13));
#23308=DIRECTION('',(-1.00515054169548E-26,1.1518563880486E-13,1.));
#23309=DIRECTION('center_axis',(1.00515054169548E-26,-1.1518563880486E-13,
-1.));
#23310=DIRECTION('ref_axis',(-8.72635297355373E-14,1.,-1.1518563880486E-13));
#23311=DIRECTION('',(1.00515054169548E-26,-1.1518563880486E-13,-1.));
#23312=DIRECTION('center_axis',(-1.,-8.67672446588636E-14,-5.71649135859828E-29));
#23313=DIRECTION('ref_axis',(-8.67672446588636E-14,1.,-1.1518563880486E-13));
#23314=DIRECTION('',(1.00515054169548E-26,-1.1518563880486E-13,-1.));
#23315=DIRECTION('',(-8.72635297355373E-14,1.,-1.1518563880486E-13));
#23316=DIRECTION('',(1.00515054169548E-26,-1.1518563880486E-13,-1.));
#23317=DIRECTION('center_axis',(-1.00515054169548E-26,1.1518563880486E-13,
1.));
#23318=DIRECTION('ref_axis',(-8.67361737988404E-14,1.,-1.1518563880486E-13));
#23319=DIRECTION('',(-1.00515054169548E-26,1.1518563880486E-13,1.));
#23320=DIRECTION('center_axis',(-1.00515054169548E-26,1.1518563880486E-13,
1.));
#23321=DIRECTION('ref_axis',(-8.67361737988404E-14,1.,-1.1518563880486E-13));
#23322=DIRECTION('center_axis',(-0.374606593415835,-0.927183854566819,1.06798264577828E-13));
#23323=DIRECTION('ref_axis',(-0.927183854566819,0.374606593415835,-4.31492997631247E-14));
#23324=DIRECTION('',(-1.00515054169548E-26,1.1518563880486E-13,1.));
#23325=DIRECTION('',(-0.92718385456682,0.374606593415832,-4.31492997631244E-14));
#23326=DIRECTION('center_axis',(8.72635297355373E-14,-1.,1.1518563880486E-13));
#23327=DIRECTION('ref_axis',(-1.00515054169548E-26,1.1518563880486E-13,
1.));
#23328=DIRECTION('',(-1.00515054169548E-26,1.1518563880486E-13,1.));
#23329=DIRECTION('',(-1.,-8.72635297355373E-14,0.));
#23330=DIRECTION('center_axis',(0.374606593415997,-0.927183854566753,1.06798264577828E-13));
#23331=DIRECTION('ref_axis',(-0.927183854566753,-0.374606593415997,4.31492997631247E-14));
#23332=DIRECTION('',(1.00515054169548E-26,-1.1518563880486E-13,-1.));
#23333=DIRECTION('',(-0.927183854566754,-0.374606593415995,4.31492997631245E-14));
#23334=DIRECTION('center_axis',(-1.00515054169548E-26,1.1518563880486E-13,
1.));
#23335=DIRECTION('ref_axis',(-8.67361737988404E-14,1.,-1.1518563880486E-13));
#23336=DIRECTION('',(-1.00515054169548E-26,1.1518563880486E-13,1.));
#23337=DIRECTION('center_axis',(-1.00515054169548E-26,1.1518563880486E-13,
1.));
#23338=DIRECTION('ref_axis',(-8.67361737988404E-14,1.,-1.1518563880486E-13));
#23339=DIRECTION('center_axis',(1.,8.7759814812211E-14,-5.71649135859828E-29));
#23340=DIRECTION('ref_axis',(8.7759814812211E-14,-1.,1.1518563880486E-13));
#23341=DIRECTION('',(8.72635297355373E-14,-1.,1.1518563880486E-13));
#23342=DIRECTION('',(-1.00515054169548E-26,1.1518563880486E-13,1.));
#23343=DIRECTION('',(8.72635297355373E-14,-1.,1.1518563880486E-13));
#23344=DIRECTION('center_axis',(1.00515054169548E-26,-1.1518563880486E-13,
-1.));
#23345=DIRECTION('ref_axis',(8.72635297355373E-14,-1.,1.1518563880486E-13));
#23346=DIRECTION('',(0.997564050259819,0.0697564737442022,-8.03494398899034E-15));
#23347=DIRECTION('',(-1.,-8.7759814812211E-14,5.71649135859831E-29));
#23348=DIRECTION('',(0.0697564737440384,0.99756405025983,-1.14905052377941E-13));
#23349=DIRECTION('center_axis',(-1.00515054169548E-26,1.1518563880486E-13,
1.));
#23350=DIRECTION('ref_axis',(-8.72635297355373E-14,1.,-1.1518563880486E-13));
#23351=DIRECTION('center_axis',(-1.00515054169548E-26,1.1518563880486E-13,
1.));
#23352=DIRECTION('ref_axis',(-8.72635297355373E-14,1.,-1.1518563880486E-13));
#23353=DIRECTION('',(-1.00515054169548E-26,1.1518563880486E-13,1.));
#23354=DIRECTION('center_axis',(1.00515054169548E-26,-1.1518563880486E-13,
-1.));
#23355=DIRECTION('ref_axis',(-9.17044218340379E-14,1.,-1.1518563880486E-13));
#23356=DIRECTION('',(1.00515054169548E-26,-1.1518563880486E-13,-1.));
#23357=DIRECTION('center_axis',(8.7759814812211E-14,-1.,1.1518563880486E-13));
#23358=DIRECTION('ref_axis',(-1.,-8.7759814812211E-14,5.71649135859828E-29));
#23359=DIRECTION('',(1.00515054169548E-26,-1.1518563880486E-13,-1.));
#23360=DIRECTION('',(-1.,-8.72635297355373E-14,0.));
#23361=DIRECTION('',(1.00515054169548E-26,-1.1518563880486E-13,-1.));
#23362=DIRECTION('center_axis',(-1.00515054169548E-26,1.1518563880486E-13,
1.));
#23363=DIRECTION('ref_axis',(-8.67361737988404E-14,1.,-1.1518563880486E-13));
#23364=DIRECTION('',(-1.00515054169548E-26,1.1518563880486E-13,1.));
#23365=DIRECTION('center_axis',(-1.00515054169548E-26,1.1518563880486E-13,
1.));
#23366=DIRECTION('ref_axis',(-8.67361737988404E-14,1.,-1.1518563880486E-13));
#23367=DIRECTION('center_axis',(0.927183854566819,-0.374606593415834,4.31492997631247E-14));
#23368=DIRECTION('ref_axis',(-0.374606593415834,-0.927183854566819,1.06798264577828E-13));
#23369=DIRECTION('',(-1.00515054169548E-26,1.1518563880486E-13,1.));
#23370=DIRECTION('',(-0.374606593415836,-0.927183854566818,1.06798264577828E-13));
#23371=DIRECTION('center_axis',(1.,8.72635297355373E-14,0.));
#23372=DIRECTION('ref_axis',(8.72635297355373E-14,-1.,1.1518563880486E-13));
#23373=DIRECTION('',(-1.00515054169548E-26,1.1518563880486E-13,1.));
#23374=DIRECTION('',(8.72635297355373E-14,-1.,1.1518563880486E-13));
#23375=DIRECTION('center_axis',(0.927183854566754,0.374606593415996,-4.31492997631246E-14));
#23376=DIRECTION('ref_axis',(0.374606593415996,-0.927183854566754,1.06798264577828E-13));
#23377=DIRECTION('',(1.00515054169548E-26,-1.1518563880486E-13,-1.));
#23378=DIRECTION('',(0.374606593415997,-0.927183854566753,1.06798264577828E-13));
#23379=DIRECTION('center_axis',(-1.00515054169548E-26,1.1518563880486E-13,
1.));
#23380=DIRECTION('ref_axis',(-8.67361737988403E-14,1.,-1.1518563880486E-13));
#23381=DIRECTION('',(-1.00515054169548E-26,1.1518563880486E-13,1.));
#23382=DIRECTION('center_axis',(-1.00515054169548E-26,1.1518563880486E-13,
1.));
#23383=DIRECTION('ref_axis',(-8.67361737988404E-14,1.,-1.1518563880486E-13));
#23384=DIRECTION('center_axis',(-8.67672446588636E-14,1.,-1.1518563880486E-13));
#23385=DIRECTION('ref_axis',(1.,8.67672446588636E-14,5.71649135859828E-29));
#23386=DIRECTION('',(1.,8.72635297355373E-14,0.));
#23387=DIRECTION('',(-1.00515054169548E-26,1.1518563880486E-13,1.));
#23388=DIRECTION('',(1.,8.72635297355373E-14,0.));
#23389=DIRECTION('center_axis',(1.00515054169548E-26,-1.1518563880486E-13,
-1.));
#23390=DIRECTION('ref_axis',(8.72635297355373E-14,-1.,1.1518563880486E-13));
#23391=DIRECTION('',(-0.0697564737442125,0.997564050259818,-1.14905052377941E-13));
#23392=DIRECTION('',(8.67672446588636E-14,-1.,1.1518563880486E-13));
#23393=DIRECTION('',(-0.997564050259831,0.0697564737440281,-8.03494398899034E-15));
#23394=DIRECTION('center_axis',(-1.00515054169548E-26,1.1518563880486E-13,
1.));
#23395=DIRECTION('ref_axis',(-8.72635297355373E-14,1.,-1.1518563880486E-13));
#23396=DIRECTION('center_axis',(-1.00515054169548E-26,1.1518563880486E-13,
1.));
#23397=DIRECTION('ref_axis',(-8.72635297355373E-14,1.,-1.1518563880486E-13));
#23398=DIRECTION('',(-1.00515054169548E-26,1.1518563880486E-13,1.));
#23399=DIRECTION('center_axis',(1.00515054169548E-26,-1.1518563880486E-13,
-1.));
#23400=DIRECTION('ref_axis',(-8.72635297355373E-14,1.,-1.1518563880486E-13));
#23401=DIRECTION('',(1.00515054169548E-26,-1.1518563880486E-13,-1.));
#23402=DIRECTION('center_axis',(1.,8.67672446588636E-14,5.71649135859828E-29));
#23403=DIRECTION('ref_axis',(8.67672446588636E-14,-1.,1.1518563880486E-13));
#23404=DIRECTION('',(1.00515054169548E-26,-1.1518563880486E-13,-1.));
#23405=DIRECTION('',(8.72635297355373E-14,-1.,1.1518563880486E-13));
#23406=DIRECTION('',(1.00515054169548E-26,-1.1518563880486E-13,-1.));
#23407=DIRECTION('center_axis',(-1.00515054169548E-26,1.1518563880486E-13,
1.));
#23408=DIRECTION('ref_axis',(-8.67361737988403E-14,1.,-1.1518563880486E-13));
#23409=DIRECTION('',(-1.00515054169548E-26,1.1518563880486E-13,1.));
#23410=DIRECTION('center_axis',(-1.00515054169548E-26,1.1518563880486E-13,
1.));
#23411=DIRECTION('ref_axis',(-8.67361737988403E-14,1.,-1.1518563880486E-13));
#23412=DIRECTION('center_axis',(0.374606593415835,0.927183854566819,-1.06798264577828E-13));
#23413=DIRECTION('ref_axis',(0.927183854566819,-0.374606593415835,4.31492997631247E-14));
#23414=DIRECTION('',(-1.00515054169548E-26,1.1518563880486E-13,1.));
#23415=DIRECTION('',(0.927183854566819,-0.374606593415834,4.31492997631246E-14));
#23416=DIRECTION('center_axis',(-8.72635297355373E-14,1.,-1.1518563880486E-13));
#23417=DIRECTION('ref_axis',(1.00515054169548E-26,-1.1518563880486E-13,
-1.));
#23418=DIRECTION('',(-1.00515054169548E-26,1.1518563880486E-13,1.));
#23419=DIRECTION('',(1.,8.72635297355373E-14,0.));
#23420=DIRECTION('center_axis',(-0.374606593415997,0.927183854566753,-1.06798264577828E-13));
#23421=DIRECTION('ref_axis',(0.927183854566753,0.374606593415997,-4.31492997631247E-14));
#23422=DIRECTION('',(1.00515054169548E-26,-1.1518563880486E-13,-1.));
#23423=DIRECTION('',(0.927183854566754,0.374606593415995,-4.31492997631245E-14));
#23424=DIRECTION('center_axis',(-1.00515054169548E-26,1.1518563880486E-13,
1.));
#23425=DIRECTION('ref_axis',(-8.67361737988403E-14,1.,-1.1518563880486E-13));
#23426=DIRECTION('',(-1.00515054169548E-26,1.1518563880486E-13,1.));
#23427=DIRECTION('center_axis',(-1.00515054169548E-26,1.1518563880486E-13,
1.));
#23428=DIRECTION('ref_axis',(-8.67361737988403E-14,1.,-1.1518563880486E-13));
#23429=DIRECTION('center_axis',(-1.,-8.7759814812211E-14,5.71649135859828E-29));
#23430=DIRECTION('ref_axis',(-8.7759814812211E-14,1.,-1.1518563880486E-13));
#23431=DIRECTION('',(-1.00515054169548E-26,1.1518563880486E-13,1.));
#23432=DIRECTION('',(-8.72635297355373E-14,1.,-1.1518563880486E-13));
#23433=DIRECTION('center_axis',(-0.342020143298471,7.83793320738915E-14,
0.939692620795808));
#23434=DIRECTION('ref_axis',(0.939692620795808,1.21396703647044E-13,0.342020143298471));
#23435=DIRECTION('',(-0.868162779198992,-0.382683432380925,-0.315985410097739));
#23436=DIRECTION('',(0.359604797523941,-0.923879532498189,0.130885442386437));
#23437=DIRECTION('',(0.868162779198971,0.382683432380902,0.315985410097825));
#23438=DIRECTION('center_axis',(0.140416818327027,-0.800103145195805,0.58319642846874));
#23439=DIRECTION('ref_axis',(-5.1390560202283E-14,0.589032278086391,0.808109507042429));
#23440=DIRECTION('',(-0.868162779198997,-0.382683432381008,-0.315985410097624));
#23441=DIRECTION('',(0.476000531462651,-0.461939766230853,-0.748354960177227));
#23442=DIRECTION('center_axis',(0.482436961612334,-0.800103145195884,-0.356496192290904));
#23443=DIRECTION('ref_axis',(-0.856369374376448,-0.516363723193343,5.94698587038405E-14));
#23444=DIRECTION('',(-0.868162779198969,-0.38268343238096,-0.315985410097759));
#23445=DIRECTION('',(0.116395733952524,0.461939766231793,-0.879240402558577));
#23446=DIRECTION('center_axis',(0.342020143298471,-7.83793320738915E-14,
-0.939692620795808));
#23447=DIRECTION('ref_axis',(-0.939692620795808,-1.21396703647044E-13,-0.342020143298471));
#23448=DIRECTION('',(-0.868162779198955,-0.382683432380959,-0.3159854100978));
#23449=DIRECTION('',(-0.359604797523941,0.923879532498189,-0.130885442386437));
#23450=DIRECTION('center_axis',(-0.140416818327027,0.800103145195805,-0.58319642846874));
#23451=DIRECTION('ref_axis',(5.1390560202283E-14,-0.589032278086391,-0.808109507042429));
#23452=DIRECTION('',(-0.86816277919896,-0.382683432380859,-0.315985410097906));
#23453=DIRECTION('',(-0.476000531462647,0.461939766230845,0.748354960177234));
#23454=DIRECTION('center_axis',(-0.482436961612334,0.800103145195884,0.356496192290904));
#23455=DIRECTION('ref_axis',(0.856369374376448,0.516363723193343,-5.94698587038405E-14));
#23456=DIRECTION('',(-0.116395733952528,-0.461939766231792,0.879240402558578));
#23457=DIRECTION('center_axis',(-8.72635297355373E-14,1.,-1.11694157466017E-13));
#23458=DIRECTION('ref_axis',(9.74682643132155E-27,-1.11694157466017E-13,
-1.));
#23459=DIRECTION('center_axis',(-8.72635297355373E-14,1.,-1.11694157466017E-13));
#23460=DIRECTION('ref_axis',(9.74682643132155E-27,-1.11694157466017E-13,
-1.));
#23461=DIRECTION('center_axis',(1.,8.72635297355373E-14,0.));
#23462=DIRECTION('ref_axis',(8.72635297355373E-14,-1.,1.1518563880486E-13));
#23463=DIRECTION('',(8.72635297355373E-14,-1.,1.1518563880486E-13));
#23464=DIRECTION('',(8.72635297355373E-14,-1.,1.1518563880486E-13));
#23465=DIRECTION('center_axis',(-1.00515054169548E-26,1.1518563880486E-13,
1.));
#23466=DIRECTION('ref_axis',(-8.72635297355373E-14,1.,-1.1518563880486E-13));
#23467=DIRECTION('',(8.72635297355373E-14,-1.,1.1518563880486E-13));
#23468=DIRECTION('center_axis',(-1.,-8.72635297355373E-14,0.));
#23469=DIRECTION('ref_axis',(-8.72635297355373E-14,1.,-1.1518563880486E-13));
#23470=DIRECTION('',(-8.72635297355373E-14,1.,-1.1518563880486E-13));
#23471=DIRECTION('center_axis',(-1.00515054169548E-26,1.1518563880486E-13,
1.));
#23472=DIRECTION('ref_axis',(-8.72635297355373E-14,1.,-1.1518563880486E-13));
#23473=DIRECTION('center_axis',(-1.00515054169548E-26,1.1518563880486E-13,
1.));
#23474=DIRECTION('ref_axis',(-8.72635297355373E-14,1.,-1.1518563880486E-13));
#23475=DIRECTION('center_axis',(-1.00515054169548E-26,1.1518563880486E-13,
1.));
#23476=DIRECTION('ref_axis',(-8.72635297355373E-14,1.,-1.1518563880486E-13));
#23477=DIRECTION('center_axis',(-1.00515054169548E-26,1.1518563880486E-13,
1.));
#23478=DIRECTION('ref_axis',(-8.72635297355373E-14,1.,-1.1518563880486E-13));
#23479=DIRECTION('center_axis',(-1.00515054169548E-26,1.1518563880486E-13,
1.));
#23480=DIRECTION('ref_axis',(-8.72635297355373E-14,1.,-1.1518563880486E-13));
#23481=DIRECTION('center_axis',(-0.0697564737442026,0.997564050259819,-1.14905052377941E-13));
#23482=DIRECTION('ref_axis',(0.997564050259819,0.0697564737442026,-8.03494398899039E-15));
#23483=DIRECTION('',(-0.997564050259819,-0.0697564737441991,8.03494398898999E-15));
#23484=DIRECTION('',(-1.00515054169548E-26,1.1518563880486E-13,1.));
#23485=DIRECTION('',(-0.997564050259819,-0.0697564737441972,8.03494398898977E-15));
#23486=DIRECTION('center_axis',(1.00515054169548E-26,-1.1518563880486E-13,
-1.));
#23487=DIRECTION('ref_axis',(8.72635297355373E-14,-1.,1.1518563880486E-13));
#23488=DIRECTION('',(0.0697564737440412,0.99756405025983,-1.14905052377941E-13));
#23489=DIRECTION('center_axis',(-1.00515054169548E-26,1.1518563880486E-13,
1.));
#23490=DIRECTION('ref_axis',(-8.72635297355373E-14,1.,-1.1518563880486E-13));
#23491=DIRECTION('',(0.997564050259818,0.0697564737442111,-8.03494398899137E-15));
#23492=DIRECTION('center_axis',(-1.00515054169548E-26,1.1518563880486E-13,
1.));
#23493=DIRECTION('ref_axis',(-8.72635297355373E-14,1.,-1.1518563880486E-13));
#23494=DIRECTION('',(0.0697564737440384,0.99756405025983,-1.14905052377941E-13));
#23495=DIRECTION('center_axis',(-1.00515054169548E-26,1.1518563880486E-13,
1.));
#23496=DIRECTION('ref_axis',(-8.72635297355373E-14,1.,-1.1518563880486E-13));
#23497=DIRECTION('center_axis',(-0.99756405025983,0.0697564737440384,-8.03494398899153E-15));
#23498=DIRECTION('ref_axis',(0.0697564737440384,0.99756405025983,-1.14905052377941E-13));
#23499=DIRECTION('',(-0.0697564737440323,-0.997564050259831,1.14905052377941E-13));
#23500=DIRECTION('',(1.00515054169548E-26,-1.1518563880486E-13,-1.));
#23501=DIRECTION('center_axis',(-1.00515054169548E-26,1.1518563880486E-13,
1.));
#23502=DIRECTION('ref_axis',(-8.72635297355373E-14,1.,-1.1518563880486E-13));
#23503=DIRECTION('',(0.0697564737442125,-0.997564050259818,1.14905052377941E-13));
#23504=DIRECTION('center_axis',(-1.00515054169548E-26,1.1518563880486E-13,
1.));
#23505=DIRECTION('ref_axis',(-8.72635297355373E-14,1.,-1.1518563880486E-13));
#23506=DIRECTION('center_axis',(-0.997564050259818,-0.0697564737442125,
8.03494398899153E-15));
#23507=DIRECTION('ref_axis',(-0.0697564737442125,0.997564050259818,-1.14905052377941E-13));
#23508=DIRECTION('',(0.0697564737442101,-0.997564050259818,1.14905052377941E-13));
#23509=DIRECTION('',(-1.00515054169548E-26,1.1518563880486E-13,1.));
#23510=DIRECTION('center_axis',(1.00515054169548E-26,-1.1518563880486E-13,
-1.));
#23511=DIRECTION('ref_axis',(8.72635297355373E-14,-1.,1.1518563880486E-13));
#23512=DIRECTION('',(-0.99756405025983,0.069756473744037,-8.03494398899137E-15));
#23513=DIRECTION('center_axis',(-1.00515054169548E-26,1.1518563880486E-13,
1.));
#23514=DIRECTION('ref_axis',(-8.72635297355373E-14,1.,-1.1518563880486E-13));
#23515=DIRECTION('',(-0.0697564737442153,0.997564050259818,-1.14905052377941E-13));
#23516=DIRECTION('center_axis',(-1.00515054169548E-26,1.1518563880486E-13,
1.));
#23517=DIRECTION('ref_axis',(-8.72635297355373E-14,1.,-1.1518563880486E-13));
#23518=DIRECTION('',(-0.997564050259831,0.0697564737440285,-8.03494398899039E-15));
#23519=DIRECTION('center_axis',(-0.0697564737440285,-0.997564050259831,
1.14905052377941E-13));
#23520=DIRECTION('ref_axis',(-0.997564050259831,0.0697564737440285,-8.03494398899039E-15));
#23521=DIRECTION('',(0.997564050259831,-0.0697564737440292,8.03494398899047E-15));
#23522=DIRECTION('center_axis',(-1.00515054169548E-26,1.1518563880486E-13,
1.));
#23523=DIRECTION('ref_axis',(-8.72635297355373E-14,1.,-1.1518563880486E-13));
#23524=DIRECTION('',(0.997564050259819,0.0697564737442022,-8.03494398899034E-15));
#23525=DIRECTION('center_axis',(0.0697564737442022,-0.997564050259819,1.14905052377941E-13));
#23526=DIRECTION('ref_axis',(-0.997564050259819,-0.0697564737442022,8.03494398899034E-15));
#23527=DIRECTION('',(0.997564050259819,0.0697564737442046,-8.03494398899062E-15));
#23528=DIRECTION('center_axis',(1.00515054169548E-26,-1.1518563880486E-13,
-1.));
#23529=DIRECTION('ref_axis',(8.72635297355373E-14,-1.,1.1518563880486E-13));
#23530=DIRECTION('',(-0.0697564737440384,-0.99756405025983,1.14905052377941E-13));
#23531=DIRECTION('center_axis',(-1.00515054169548E-26,1.1518563880486E-13,
1.));
#23532=DIRECTION('ref_axis',(-8.72635297355373E-14,1.,-1.1518563880486E-13));
#23533=DIRECTION('',(-0.0697564737440412,-0.99756405025983,1.14905052377941E-13));
#23534=DIRECTION('center_axis',(-1.00515054169548E-26,1.1518563880486E-13,
1.));
#23535=DIRECTION('ref_axis',(-8.72635297355373E-14,1.,-1.1518563880486E-13));
#23536=DIRECTION('',(-0.997564050259818,-0.0697564737442111,8.03494398899137E-15));
#23537=DIRECTION('center_axis',(0.99756405025983,-0.0697564737440384,8.03494398899153E-15));
#23538=DIRECTION('ref_axis',(-0.0697564737440384,-0.99756405025983,1.14905052377941E-13));
#23539=DIRECTION('',(0.0697564737440399,0.99756405025983,-1.14905052377941E-13));
#23540=DIRECTION('',(1.00515054169548E-26,-1.1518563880486E-13,-1.));
#23541=DIRECTION('center_axis',(-1.00515054169548E-26,1.1518563880486E-13,
1.));
#23542=DIRECTION('ref_axis',(-8.72635297355373E-14,1.,-1.1518563880486E-13));
#23543=DIRECTION('',(-0.0697564737442125,0.997564050259818,-1.14905052377941E-13));
#23544=DIRECTION('center_axis',(-1.00515054169548E-26,1.1518563880486E-13,
1.));
#23545=DIRECTION('ref_axis',(-8.72635297355373E-14,1.,-1.1518563880486E-13));
#23546=DIRECTION('center_axis',(0.997564050259818,0.0697564737442125,-8.03494398899153E-15));
#23547=DIRECTION('ref_axis',(0.0697564737442125,-0.997564050259818,1.14905052377941E-13));
#23548=DIRECTION('',(-0.0697564737442101,0.997564050259818,-1.14905052377941E-13));
#23549=DIRECTION('',(-1.00515054169548E-26,1.1518563880486E-13,1.));
#23550=DIRECTION('center_axis',(1.00515054169548E-26,-1.1518563880486E-13,
-1.));
#23551=DIRECTION('ref_axis',(8.72635297355373E-14,-1.,1.1518563880486E-13));
#23552=DIRECTION('',(0.997564050259831,-0.0697564737440281,8.03494398899034E-15));
#23553=DIRECTION('center_axis',(-1.00515054169548E-26,1.1518563880486E-13,
1.));
#23554=DIRECTION('ref_axis',(-8.72635297355373E-14,1.,-1.1518563880486E-13));
#23555=DIRECTION('',(0.99756405025983,-0.069756473744037,8.03494398899137E-15));
#23556=DIRECTION('center_axis',(-1.00515054169548E-26,1.1518563880486E-13,
1.));
#23557=DIRECTION('ref_axis',(-8.72635297355373E-14,1.,-1.1518563880486E-13));
#23558=DIRECTION('',(0.0697564737442153,-0.997564050259818,1.14905052377941E-13));
#23559=DIRECTION('center_axis',(-1.00515054169548E-26,1.1518563880486E-13,
1.));
#23560=DIRECTION('ref_axis',(-8.72635297355373E-14,1.,-1.1518563880486E-13));
#23561=DIRECTION('center_axis',(0.0697564737440281,0.997564050259831,-1.14905052377941E-13));
#23562=DIRECTION('ref_axis',(0.997564050259831,-0.0697564737440281,8.03494398899034E-15));
#23563=DIRECTION('',(-0.997564050259831,0.0697564737440302,-8.03494398899059E-15));
#23564=DIRECTION('',(1.00515054169548E-26,-1.1518563880486E-13,-1.));
#23565=DIRECTION('center_axis',(-1.00515054169548E-26,1.1518563880486E-13,
1.));
#23566=DIRECTION('ref_axis',(-8.72635297355373E-14,1.,-1.1518563880486E-13));
#23567=DIRECTION('center_axis',(-1.00515054169548E-26,1.1518563880486E-13,
1.));
#23568=DIRECTION('ref_axis',(-8.72635297355373E-14,1.,-1.1518563880486E-13));
#23569=DIRECTION('center_axis',(-0.868162779192245,-0.38268343239671,-0.315985410097158));
#23570=DIRECTION('ref_axis',(-0.403349423721026,0.915046032931631,-1.05414319346039E-13));
#23571=DIRECTION('center_axis',(-8.72635297355373E-14,1.,-1.11694157466017E-13));
#23572=DIRECTION('ref_axis',(9.74682643132155E-27,-1.11694157466017E-13,
-1.));
#23573=DIRECTION('',(0.5,-5.61219244883788E-14,-0.866025403784439));
#23574=DIRECTION('',(-0.5,-1.43385454223916E-13,-0.866025403784438));
#23575=DIRECTION('',(-1.,-8.72635297355373E-14,0.));
#23576=DIRECTION('',(-0.5,5.61219244883788E-14,0.866025403784439));
#23577=DIRECTION('',(0.5,1.43385454223916E-13,0.866025403784439));
#23578=DIRECTION('',(1.,8.72635297355373E-14,-1.21904419394898E-29));
#23579=DIRECTION('center_axis',(0.0697564737442111,-0.997564050259818,1.14905052377941E-13));
#23580=DIRECTION('ref_axis',(-0.997564050259818,-0.0697564737442111,8.03494398899137E-15));
#23581=DIRECTION('',(1.00515054169548E-26,-1.1518563880486E-13,-1.));
#23582=DIRECTION('',(1.00515054169548E-26,-1.1518563880486E-13,-1.));
#23583=DIRECTION('center_axis',(-1.00515054169548E-26,1.1518563880486E-13,
1.));
#23584=DIRECTION('ref_axis',(-8.72635297355373E-14,1.,-1.1518563880486E-13));
#23585=DIRECTION('',(1.00515054169548E-26,-1.1518563880486E-13,-1.));
#23586=DIRECTION('center_axis',(0.99756405025983,-0.0697564737440412,8.03494398899185E-15));
#23587=DIRECTION('ref_axis',(-0.0697564737440412,-0.99756405025983,1.14905052377941E-13));
#23588=DIRECTION('',(1.00515054169548E-26,-1.1518563880486E-13,-1.));
#23589=DIRECTION('center_axis',(-1.00515054169548E-26,1.1518563880486E-13,
1.));
#23590=DIRECTION('ref_axis',(-8.72635297355373E-14,1.,-1.1518563880486E-13));
#23591=DIRECTION('',(1.00515054169548E-26,-1.1518563880486E-13,-1.));
#23592=DIRECTION('center_axis',(0.997564050259818,0.0697564737442153,-8.03494398899185E-15));
#23593=DIRECTION('ref_axis',(0.0697564737442153,-0.997564050259818,1.14905052377941E-13));
#23594=DIRECTION('',(1.00515054169548E-26,-1.1518563880486E-13,-1.));
#23595=DIRECTION('center_axis',(-1.00515054169548E-26,1.1518563880486E-13,
1.));
#23596=DIRECTION('ref_axis',(-8.72635297355373E-14,1.,-1.1518563880486E-13));
#23597=DIRECTION('',(1.00515054169548E-26,-1.1518563880486E-13,-1.));
#23598=DIRECTION('center_axis',(0.069756473744037,0.99756405025983,-1.14905052377941E-13));
#23599=DIRECTION('ref_axis',(0.99756405025983,-0.069756473744037,8.03494398899137E-15));
#23600=DIRECTION('center_axis',(-0.0697564737442111,0.997564050259818,-1.14905052377941E-13));
#23601=DIRECTION('ref_axis',(0.997564050259818,0.0697564737442111,-8.03494398899137E-15));
#23602=DIRECTION('',(1.00515054169548E-26,-1.1518563880486E-13,-1.));
#23603=DIRECTION('center_axis',(-1.00515054169548E-26,1.1518563880486E-13,
1.));
#23604=DIRECTION('ref_axis',(-8.72635297355373E-14,1.,-1.1518563880486E-13));
#23605=DIRECTION('',(1.00515054169548E-26,-1.1518563880486E-13,-1.));
#23606=DIRECTION('center_axis',(-0.99756405025983,0.0697564737440412,-8.03494398899185E-15));
#23607=DIRECTION('ref_axis',(0.0697564737440412,0.99756405025983,-1.14905052377941E-13));
#23608=DIRECTION('',(1.00515054169548E-26,-1.1518563880486E-13,-1.));
#23609=DIRECTION('center_axis',(-1.00515054169548E-26,1.1518563880486E-13,
1.));
#23610=DIRECTION('ref_axis',(-8.72635297355373E-14,1.,-1.1518563880486E-13));
#23611=DIRECTION('',(1.00515054169548E-26,-1.1518563880486E-13,-1.));
#23612=DIRECTION('center_axis',(-0.997564050259818,-0.0697564737442153,
8.03494398899185E-15));
#23613=DIRECTION('ref_axis',(-0.0697564737442153,0.997564050259818,-1.14905052377941E-13));
#23614=DIRECTION('',(1.00515054169548E-26,-1.1518563880486E-13,-1.));
#23615=DIRECTION('center_axis',(-1.00515054169548E-26,1.1518563880486E-13,
1.));
#23616=DIRECTION('ref_axis',(-8.72635297355373E-14,1.,-1.1518563880486E-13));
#23617=DIRECTION('',(1.00515054169548E-26,-1.1518563880486E-13,-1.));
#23618=DIRECTION('center_axis',(-0.069756473744037,-0.99756405025983,1.14905052377941E-13));
#23619=DIRECTION('ref_axis',(-0.99756405025983,0.069756473744037,-8.03494398899137E-15));
#23620=DIRECTION('',(1.00515054169548E-26,-1.1518563880486E-13,-1.));
#23621=DIRECTION('center_axis',(-1.00515054169548E-26,1.1518563880486E-13,
1.));
#23622=DIRECTION('ref_axis',(8.71410650556226E-14,-1.,1.1518563880486E-13));
#23623=DIRECTION('center_axis',(8.72635297355373E-14,-1.,1.1518563880486E-13));
#23624=DIRECTION('ref_axis',(-1.,-8.72635297355373E-14,-1.43492962746861E-42));
#23625=DIRECTION('',(-1.,-8.72635297355373E-14,0.));
#23626=DIRECTION('',(-1.,-8.72635297355373E-14,0.));
#23627=DIRECTION('',(-1.00515054169548E-26,1.1518563880486E-13,1.));
#23628=DIRECTION('',(1.,8.72635297355373E-14,2.47817639425246E-16));
#23629=DIRECTION('',(1.,8.72635297355373E-14,2.47817639425246E-16));
#23630=DIRECTION('',(1.,8.72635297355373E-14,1.40416384211369E-42));
#23631=DIRECTION('',(1.65211759626891E-16,-1.1518563880486E-13,-1.));
#23632=DIRECTION('',(-1.,-8.72635297355373E-14,0.));
#23633=DIRECTION('center_axis',(2.47817639435298E-16,-1.1518563880486E-13,
-1.));
#23634=DIRECTION('ref_axis',(-1.,-8.72635297355373E-14,-2.47817639425246E-16));
#23635=DIRECTION('center_axis',(9.74874922969709E-27,-1.11716191852906E-13,
-1.));
#23636=DIRECTION('ref_axis',(8.73144149574993E-14,-1.,1.11716191852906E-13));
#23637=DIRECTION('center_axis',(9.74874922969709E-27,-1.11716191852906E-13,
-1.));
#23638=DIRECTION('ref_axis',(8.73144149574993E-14,-1.,1.11716191852906E-13));
#23639=DIRECTION('center_axis',(-9.74682643132153E-27,1.11694157466017E-13,
1.));
#23640=DIRECTION('ref_axis',(-8.72635297355373E-14,1.,-1.11694157466017E-13));
#23641=DIRECTION('center_axis',(-9.74874922969709E-27,1.11716191852906E-13,
1.));
#23642=DIRECTION('ref_axis',(9.07838619094529E-14,-1.,1.11716191852906E-13));
#23643=DIRECTION('',(1.,8.72635297355373E-14,0.));
#23644=DIRECTION('center_axis',(-9.74874922969709E-27,1.11716191852906E-13,
1.));
#23645=DIRECTION('ref_axis',(8.38449680055457E-14,-1.,1.11716191852906E-13));
#23646=DIRECTION('center_axis',(-8.72635297355373E-14,1.,-1.11694157466017E-13));
#23647=DIRECTION('ref_axis',(9.74682643132155E-27,-1.11694157466017E-13,
-1.));
#23648=DIRECTION('',(6.60847038457304E-16,1.1518563880486E-13,1.));
#23649=DIRECTION('',(1.,8.72635297355373E-14,-1.21904419394898E-29));
#23650=DIRECTION('',(1.,8.72635297355373E-14,-1.21904419394898E-29));
#23651=DIRECTION('',(-1.,-8.72635297355373E-14,0.));
#23652=DIRECTION('',(6.60847038477406E-16,-1.1518563880486E-13,-1.));
#23653=DIRECTION('',(-1.,-8.72635297355373E-14,0.));
#23654=DIRECTION('',(-1.,-8.72635297355373E-14,0.));
#23655=DIRECTION('center_axis',(-8.72635297355373E-14,1.,-1.11694157466017E-13));
#23656=DIRECTION('ref_axis',(9.74682643132155E-27,-1.11694157466017E-13,
-1.));
#23657=DIRECTION('',(0.5,-5.61219244883788E-14,-0.866025403784439));
#23658=DIRECTION('',(-0.5,-1.43385454223916E-13,-0.866025403784439));
#23659=DIRECTION('',(-1.,-8.72635297355373E-14,0.));
#23660=DIRECTION('',(-0.5,5.61219244883788E-14,0.866025403784439));
#23661=DIRECTION('',(0.5,1.43385454223916E-13,0.866025403784439));
#23662=DIRECTION('',(1.,8.72635297355373E-14,-1.21904419394898E-29));
#23663=DIRECTION('center_axis',(9.74874922969709E-27,-1.11716191852906E-13,
-1.));
#23664=DIRECTION('ref_axis',(1.28885450781528E-13,1.,-1.11716191852906E-13));
#23665=DIRECTION('center_axis',(0.866025403784439,1.97253548418657E-14,
-0.5));
#23666=DIRECTION('ref_axis',(-0.5,-1.43385454223916E-13,-0.866025403784439));
#23667=DIRECTION('',(8.57516739673986E-14,-1.,1.14312768470149E-13));
#23668=DIRECTION('',(0.500000000000001,1.43385454223916E-13,0.866025403784438));
#23669=DIRECTION('',(-8.72635297355373E-14,1.,-1.1518563880486E-13));
#23670=DIRECTION('center_axis',(1.00393149750153E-26,-1.1518563880486E-13,
-1.));
#23671=DIRECTION('ref_axis',(-1.,-8.72635297355373E-14,1.219044193949E-29));
#23672=DIRECTION('',(1.,8.72635297355373E-14,1.40416384211369E-42));
#23673=DIRECTION('',(-8.57516739673986E-14,1.,-1.14312768470149E-13));
#23674=DIRECTION('center_axis',(-0.866025403784439,-1.31419512307882E-13,
-0.5));
#23675=DIRECTION('ref_axis',(-0.5,5.61219244883788E-14,0.866025403784439));
#23676=DIRECTION('',(0.500000000000001,-5.61219244883783E-14,-0.866025403784438));
#23677=DIRECTION('',(-8.8775385503676E-14,1.,-1.14312768470149E-13));
#23678=DIRECTION('center_axis',(-0.866025403784438,-1.97253548418655E-14,
0.5));
#23679=DIRECTION('ref_axis',(0.5,1.43385454223916E-13,0.866025403784438));
#23680=DIRECTION('',(-0.5,-1.43385454223916E-13,-0.866025403784438));
#23681=DIRECTION('',(-8.72635297355373E-14,1.,-1.11694157466017E-13));
#23682=DIRECTION('center_axis',(-9.74682643132153E-27,1.11694157466017E-13,
1.));
#23683=DIRECTION('ref_axis',(-8.72635297355373E-14,1.,-1.11694157466017E-13));
#23684=DIRECTION('',(-1.,-8.72635297355373E-14,-1.40416384211369E-42));
#23685=DIRECTION('',(-8.57516739673986E-14,1.,-1.14312768470149E-13));
#23686=DIRECTION('center_axis',(0.866025403784439,1.31419512307882E-13,
0.5));
#23687=DIRECTION('ref_axis',(0.5,-5.61219244883788E-14,-0.866025403784439));
#23688=DIRECTION('',(-0.5,5.61219244883785E-14,0.866025403784438));
#23689=DIRECTION('center_axis',(-8.72635297355373E-14,1.,-1.11716191852906E-13));
#23690=DIRECTION('ref_axis',(-1.89882151931492E-15,1.11716191852906E-13,
1.));
#23691=DIRECTION('',(-8.57516739673986E-14,1.,-1.14312768470149E-13));
#23692=DIRECTION('center_axis',(8.72635297355373E-14,-1.,1.11716191852906E-13));
#23693=DIRECTION('ref_axis',(-1.77809156287629E-15,-1.11716191852907E-13,
-1.));
#23694=DIRECTION('',(8.87753855036761E-14,-1.,1.14312768470149E-13));
#23695=DIRECTION('center_axis',(1.00393149750153E-26,-1.1518563880486E-13,
-1.));
#23696=DIRECTION('ref_axis',(-1.,-8.72635297355373E-14,1.219044193949E-29));
#23697=DIRECTION('center_axis',(9.74874922969709E-27,-1.11716191852906E-13,
-1.));
#23698=DIRECTION('ref_axis',(8.73144149574993E-14,-1.,1.11716191852906E-13));
#23699=DIRECTION('center_axis',(9.74874922969709E-27,-1.11716191852906E-13,
-1.));
#23700=DIRECTION('ref_axis',(8.73144149574993E-14,-1.,1.11716191852906E-13));
#23701=DIRECTION('center_axis',(-1.00515054169548E-26,1.1518563880486E-13,
1.));
#23702=DIRECTION('ref_axis',(-8.72635297355373E-14,1.,-1.1518563880486E-13));
#23703=DIRECTION('center_axis',(1.00515054169548E-26,-1.1518563880486E-13,
-1.));
#23704=DIRECTION('ref_axis',(8.72635297355373E-14,-1.,1.1518563880486E-13));
#23705=DIRECTION('center_axis',(1.00515054169548E-26,-1.1518563880486E-13,
-1.));
#23706=DIRECTION('ref_axis',(8.72635297355373E-14,-1.,1.1518563880486E-13));
#23707=DIRECTION('center_axis',(1.00515054169548E-26,-1.1518563880486E-13,
-1.));
#23708=DIRECTION('ref_axis',(8.72635297355373E-14,-1.,1.1518563880486E-13));
#23709=DIRECTION('center_axis',(1.00515054169548E-26,-1.1518563880486E-13,
-1.));
#23710=DIRECTION('ref_axis',(8.72635297355373E-14,-1.,1.1518563880486E-13));
#23711=DIRECTION('center_axis',(0.868162779192246,0.38268343239671,0.315985410097158));
#23712=DIRECTION('ref_axis',(-0.0151045175936891,0.656788415924971,-0.753923623621802));
#23713=DIRECTION('center_axis',(-0.868162779195953,-0.359604797490619,-0.342020143325637));
#23714=DIRECTION('ref_axis',(0.0151045173766889,0.669702935899703,-0.742475475151965));
#23715=DIRECTION('center_axis',(-0.868162779192246,-0.38268343239671,-0.315985410097158));
#23716=DIRECTION('ref_axis',(0.403349423721026,-0.915046032931631,1.05237388736238E-13));
#23717=DIRECTION('center_axis',(0.868162779192245,0.38268343239671,0.315985410097158));
#23718=DIRECTION('ref_axis',(0.403349423721026,-0.915046032931631,1.05414319346039E-13));
#23719=DIRECTION('',(0.496049637005668,-0.649755621195856,-0.575979505148345));
#23720=DIRECTION('',(0.496049637005668,-0.649755621195843,-0.57597950514836));
#23721=DIRECTION('center_axis',(1.,8.72635297355373E-14,0.));
#23722=DIRECTION('ref_axis',(8.72635297355373E-14,-1.,1.1518563880486E-13));
#23723=DIRECTION('',(4.36317648660808E-14,-0.499999999980658,0.866025403795606));
#23724=DIRECTION('',(-4.36317648660983E-14,0.499999999980858,0.86602540379549));
#23725=DIRECTION('',(-8.72635297355373E-14,1.,-1.1518563880486E-13));
#23726=DIRECTION('',(-4.36317648660808E-14,0.499999999980658,-0.866025403795606));
#23727=DIRECTION('',(4.36317648660983E-14,-0.499999999980858,-0.86602540379549));
#23728=DIRECTION('',(8.72635297355373E-14,-1.,1.1518563880486E-13));
#23729=DIRECTION('center_axis',(-8.72635297355373E-14,1.,-1.11694157466017E-13));
#23730=DIRECTION('ref_axis',(9.74682643132155E-27,-1.11694157466017E-13,
-1.));
#23731=DIRECTION('',(0.5,-5.61219244883788E-14,-0.866025403784439));
#23732=DIRECTION('',(-0.5,-1.43385454223916E-13,-0.866025403784438));
#23733=DIRECTION('',(-1.,-8.72635297355372E-14,1.20185167898972E-15));
#23734=DIRECTION('',(-0.5,5.61219244883789E-14,0.866025403784439));
#23735=DIRECTION('',(0.5,1.43385454223916E-13,0.866025403784439));
#23736=DIRECTION('',(1.,8.72635297355373E-14,-1.21904419394898E-29));
#23737=DIRECTION('center_axis',(-8.72635297355373E-14,1.,-1.11694157466017E-13));
#23738=DIRECTION('ref_axis',(9.74682643132155E-27,-1.11694157466017E-13,
-1.));
#23739=DIRECTION('',(0.5,-5.61219244883789E-14,-0.866025403784439));
#23740=DIRECTION('',(-0.5,-1.43385454223916E-13,-0.866025403784438));
#23741=DIRECTION('',(-1.,-8.72635297355373E-14,0.));
#23742=DIRECTION('',(-0.499999999999999,5.6121924488379E-14,0.866025403784439));
#23743=DIRECTION('',(0.5,1.43385454223916E-13,0.866025403784438));
#23744=DIRECTION('',(1.,8.72635297355373E-14,-1.21904419394898E-29));
#23745=DIRECTION('center_axis',(1.00393149750153E-26,-1.1518563880486E-13,
-1.));
#23746=DIRECTION('ref_axis',(-1.,-8.72635297355373E-14,1.219044193949E-29));
#23747=DIRECTION('center_axis',(9.74874922969709E-27,-1.11716191852906E-13,
-1.));
#23748=DIRECTION('ref_axis',(8.73144149574993E-14,-1.,1.11716191852906E-13));
#23749=DIRECTION('',(-8.72635297355373E-14,1.,-1.1518563880486E-13));
#23750=DIRECTION('center_axis',(1.,8.72635297355372E-14,-6.60847038467355E-16));
#23751=DIRECTION('ref_axis',(-6.60847038457304E-16,-1.1518563880486E-13,
-1.));
#23752=DIRECTION('',(-8.72635297355373E-14,1.,-1.11694157466017E-13));
#23753=DIRECTION('',(-9.74874922969709E-27,1.11716191852906E-13,1.));
#23754=DIRECTION('center_axis',(-9.74682643132153E-27,1.11694157466017E-13,
1.));
#23755=DIRECTION('ref_axis',(-8.72635297355373E-14,1.,-1.11694157466017E-13));
#23756=DIRECTION('center_axis',(-9.74874922969709E-27,1.11716191852906E-13,
1.));
#23757=DIRECTION('ref_axis',(8.73144149574993E-14,-1.,1.11716191852906E-13));
#23758=DIRECTION('center_axis',(2.47817639435298E-16,-1.1518563880486E-13,
-1.));
#23759=DIRECTION('ref_axis',(-1.,-8.72635297355373E-14,-2.47817639425246E-16));
#23760=DIRECTION('center_axis',(9.74874922969709E-27,-1.11716191852906E-13,
-1.));
#23761=DIRECTION('ref_axis',(8.73144149574993E-14,-1.,1.11716191852906E-13));
#23762=DIRECTION('',(-8.72635297355373E-14,1.,-1.1518563880486E-13));
#23763=DIRECTION('center_axis',(1.,8.72635297355373E-14,0.));
#23764=DIRECTION('ref_axis',(8.72635297355373E-14,-1.,1.1518563880486E-13));
#23765=DIRECTION('',(-8.72635297355373E-14,1.,-1.11694157466017E-13));
#23766=DIRECTION('',(-9.74874922969709E-27,1.11716191852906E-13,1.));
#23767=DIRECTION('center_axis',(-9.74682643132153E-27,1.11694157466017E-13,
1.));
#23768=DIRECTION('ref_axis',(-8.72635297355373E-14,1.,-1.11694157466017E-13));
#23769=DIRECTION('center_axis',(-9.74874922969709E-27,1.11716191852906E-13,
1.));
#23770=DIRECTION('ref_axis',(7.63278329429795E-14,-1.,1.11716191852906E-13));
#23771=DIRECTION('center_axis',(-9.74682643132153E-27,1.11694157466017E-13,
1.));
#23772=DIRECTION('ref_axis',(-8.72635297355373E-14,1.,-1.11694157466017E-13));
#23773=DIRECTION('center_axis',(-9.74874922969709E-27,1.11716191852906E-13,
1.));
#23774=DIRECTION('ref_axis',(8.73144149574993E-14,-1.,1.11716191852906E-13));
#23775=DIRECTION('center_axis',(-9.74874922969709E-27,1.11716191852906E-13,
1.));
#23776=DIRECTION('ref_axis',(8.73144149574993E-14,-1.,1.11716191852906E-13));
#23777=DIRECTION('center_axis',(-9.74682643132153E-27,1.11694157466017E-13,
1.));
#23778=DIRECTION('ref_axis',(-8.72635297355373E-14,1.,-1.11694157466017E-13));
#23779=DIRECTION('center_axis',(-9.74874922969709E-27,1.11716191852906E-13,
1.));
#23780=DIRECTION('ref_axis',(8.73144149574993E-14,-1.,1.11716191852906E-13));
#23781=DIRECTION('',(-8.72635297355373E-14,1.,-1.1518563880486E-13));
#23782=DIRECTION('center_axis',(-1.,-8.72635297355373E-14,-1.65211759616839E-16));
#23783=DIRECTION('ref_axis',(-1.65211759626891E-16,1.1518563880486E-13,
1.));
#23784=DIRECTION('',(-8.72635297355373E-14,1.,-1.1518563880486E-13));
#23785=DIRECTION('',(9.74874922969709E-27,-1.11716191852906E-13,-1.));
#23786=DIRECTION('center_axis',(2.47817639435298E-16,-1.1518563880486E-13,
-1.));
#23787=DIRECTION('ref_axis',(-1.,-8.72635297355373E-14,-2.47817639425246E-16));
#23788=DIRECTION('center_axis',(9.74874922969709E-27,-1.11716191852906E-13,
-1.));
#23789=DIRECTION('ref_axis',(8.73144149574993E-14,-1.,1.11716191852906E-13));
#23790=DIRECTION('center_axis',(-9.74682643132153E-27,1.11694157466017E-13,
1.));
#23791=DIRECTION('ref_axis',(-8.72635297355373E-14,1.,-1.11694157466017E-13));
#23792=DIRECTION('center_axis',(-9.74874922969709E-27,1.11716191852906E-13,
1.));
#23793=DIRECTION('ref_axis',(8.73144149574993E-14,-1.,1.11716191852906E-13));
#23794=DIRECTION('',(-8.72635297355373E-14,1.,-1.1518563880486E-13));
#23795=DIRECTION('center_axis',(-1.,-8.72635297355374E-14,-6.60847038467355E-16));
#23796=DIRECTION('ref_axis',(-6.60847038477406E-16,1.1518563880486E-13,
1.));
#23797=DIRECTION('',(-8.72635297355373E-14,1.,-1.1518563880486E-13));
#23798=DIRECTION('',(9.74874922969709E-27,-1.11716191852906E-13,-1.));
#23799=DIRECTION('center_axis',(1.00393149750153E-26,-1.1518563880486E-13,
-1.));
#23800=DIRECTION('ref_axis',(-1.,-8.72635297355373E-14,1.219044193949E-29));
#23801=DIRECTION('center_axis',(9.74874922969709E-27,-1.11716191852906E-13,
-1.));
#23802=DIRECTION('ref_axis',(8.73144149574993E-14,-1.,1.11716191852906E-13));
#23803=DIRECTION('center_axis',(0.866025403784439,1.97253548418657E-14,
-0.5));
#23804=DIRECTION('ref_axis',(-0.5,-1.43385454223916E-13,-0.866025403784439));
#23805=DIRECTION('',(8.57516739673986E-14,-1.,1.14312768470149E-13));
#23806=DIRECTION('',(-0.5,-1.40981750865937E-13,-0.866025403784439));
#23807=DIRECTION('',(-8.72635297355373E-14,1.,-1.1518563880486E-13));
#23808=DIRECTION('center_axis',(0.866025403784439,1.31419512307882E-13,
0.5));
#23809=DIRECTION('ref_axis',(0.5,-5.61219244883788E-14,-0.866025403784439));
#23810=DIRECTION('',(8.72635297355373E-14,-1.,1.11694157466017E-13));
#23811=DIRECTION('',(0.5,-5.37182211303994E-14,-0.866025403784439));
#23812=DIRECTION('center_axis',(-9.74682643132153E-27,1.11694157466017E-13,
1.));
#23813=DIRECTION('ref_axis',(-8.72635297355373E-14,1.,-1.11694157466017E-13));
#23814=DIRECTION('',(8.87753855036761E-14,-1.,1.14312768470149E-13));
#23815=DIRECTION('',(1.,8.72635297355373E-14,0.));
#23816=DIRECTION('center_axis',(-0.866025403784439,-1.97253548418657E-14,
0.5));
#23817=DIRECTION('ref_axis',(0.5,1.43385454223916E-13,0.866025403784439));
#23818=DIRECTION('',(8.57516739673986E-14,-1.,1.14312768470149E-13));
#23819=DIRECTION('',(0.5,1.40981750865937E-13,0.866025403784438));
#23820=DIRECTION('center_axis',(-0.866025403784439,-1.31419512307882E-13,
-0.5));
#23821=DIRECTION('ref_axis',(-0.5,5.61219244883788E-14,0.866025403784439));
#23822=DIRECTION('',(8.72635297355373E-14,-1.,1.1518563880486E-13));
#23823=DIRECTION('',(-0.5,5.37182211303995E-14,0.866025403784439));
#23824=DIRECTION('center_axis',(1.00393149750153E-26,-1.1518563880486E-13,
-1.));
#23825=DIRECTION('ref_axis',(-1.,-8.72635297355373E-14,1.219044193949E-29));
#23826=DIRECTION('',(-1.,-8.72635297355373E-14,0.));
#23827=DIRECTION('center_axis',(0.866025403784439,1.97253548418657E-14,
-0.5));
#23828=DIRECTION('ref_axis',(-0.5,-1.43385454223916E-13,-0.866025403784439));
#23829=DIRECTION('center_axis',(-0.866025403784486,6.32642106711312E-14,
0.499999999999918));
#23830=DIRECTION('ref_axis',(0.499999999999918,-1.40512606311845E-10,0.866025403784486));
#23831=DIRECTION('',(-0.500000000000001,-1.43385454223916E-13,-0.866025403784438));
#23832=DIRECTION('',(8.72635297355373E-14,-1.,1.11716191852906E-13));
#23833=DIRECTION('center_axis',(-8.72635297355373E-14,1.,-1.11716191852906E-13));
#23834=DIRECTION('ref_axis',(6.05512374515455E-29,-1.11716191852906E-13,
-1.));
#23835=DIRECTION('center_axis',(-8.72635297355373E-14,1.,-1.11716191852906E-13));
#23836=DIRECTION('ref_axis',(6.05512374515455E-29,-1.11716191852906E-13,
-1.));
#23837=DIRECTION('center_axis',(8.72635297355373E-14,-1.,1.1518563880486E-13));
#23838=DIRECTION('ref_axis',(-1.,-8.72635297355373E-14,-1.43492962746861E-42));
#23839=DIRECTION('',(-0.5,5.61219244883788E-14,0.866025403784439));
#23840=DIRECTION('center_axis',(-8.72635297355373E-14,1.,-1.11716191852906E-13));
#23841=DIRECTION('ref_axis',(6.05512374515455E-29,-1.11716191852906E-13,
-1.));
#23842=DIRECTION('',(1.,8.69744091562078E-14,3.23084885458356E-29));
#23843=DIRECTION('center_axis',(-8.72635297355373E-14,1.,-1.11716191852906E-13));
#23844=DIRECTION('ref_axis',(6.05512374515455E-29,-1.11716191852906E-13,
-1.));
#23845=DIRECTION('',(8.57516739673986E-14,-1.,1.14312768470149E-13));
#23846=DIRECTION('center_axis',(-0.866025403784439,-1.31419512307882E-13,
-0.5));
#23847=DIRECTION('ref_axis',(-0.5,5.61219244883788E-14,0.866025403784439));
#23848=DIRECTION('center_axis',(0.866025403784523,-8.63609033881368E-13,
0.499999999999854));
#23849=DIRECTION('ref_axis',(0.499999999999854,4.79670877767529E-10,-0.866025403784523));
#23850=DIRECTION('center_axis',(0.866025403784434,1.17391797327623E-13,
0.500000000000008));
#23851=DIRECTION('ref_axis',(0.500000000000008,-2.53120997629797E-11,-0.866025403784434));
#23852=DIRECTION('center_axis',(-8.72635297355373E-14,1.,-1.11694157466017E-13));
#23853=DIRECTION('ref_axis',(9.74682643132155E-27,-1.11694157466017E-13,
-1.));
#23854=DIRECTION('',(0.5,-5.61219244883789E-14,-0.866025403784439));
#23855=DIRECTION('',(-0.5,-1.43385454223916E-13,-0.866025403784439));
#23856=DIRECTION('',(-1.,-8.72635297355373E-14,0.));
#23857=DIRECTION('',(-0.5,5.61219244883788E-14,0.866025403784439));
#23858=DIRECTION('',(0.5,1.43385454223916E-13,0.866025403784439));
#23859=DIRECTION('',(1.,8.72635297355373E-14,-1.21904419394898E-29));
#23860=DIRECTION('center_axis',(-8.72635297355373E-14,1.,-1.11694157466017E-13));
#23861=DIRECTION('ref_axis',(9.74682643132155E-27,-1.11694157466017E-13,
-1.));
#23862=DIRECTION('',(0.5,-5.61219244883788E-14,-0.866025403784439));
#23863=DIRECTION('',(-0.5,-1.43385454223916E-13,-0.866025403784438));
#23864=DIRECTION('',(-1.,-8.72635297355373E-14,0.));
#23865=DIRECTION('',(-0.499999999999999,5.6121924488379E-14,0.866025403784439));
#23866=DIRECTION('',(0.5,1.43385454223916E-13,0.866025403784439));
#23867=DIRECTION('',(1.,8.72635297355373E-14,-1.21904419394898E-29));
#23868=DIRECTION('center_axis',(1.,8.72635297355373E-14,0.));
#23869=DIRECTION('ref_axis',(8.72635297355373E-14,-1.,1.1518563880486E-13));
#23870=DIRECTION('',(4.36317648660983E-14,-0.499999999980858,-0.86602540379549));
#23871=DIRECTION('',(-4.36317648660808E-14,0.499999999980658,-0.866025403795606));
#23872=DIRECTION('',(-8.72635297355373E-14,1.,-1.1518563880486E-13));
#23873=DIRECTION('',(-4.36317648660983E-14,0.499999999980858,0.86602540379549));
#23874=DIRECTION('',(4.36317648660808E-14,-0.499999999980658,0.866025403795606));
#23875=DIRECTION('',(8.72635297355373E-14,-1.,1.1518563880486E-13));
#23876=DIRECTION('center_axis',(0.382683432365171,-0.923879532511253,1.06417654131048E-13));
#23877=DIRECTION('ref_axis',(-0.923879532511253,-0.382683432365171,4.40796356170094E-14));
#23878=DIRECTION('',(-0.923879532511252,-0.382683432365173,4.40796356170097E-14));
#23879=DIRECTION('',(0.315985410125154,0.130885442385788,-0.939692620785922));
#23880=DIRECTION('center_axis',(0.868162779195958,0.359604797490614,0.34202014332563));
#23881=DIRECTION('ref_axis',(0.382683432365172,-0.923879532511253,1.06407127951475E-13));
#23882=DIRECTION('',(-0.382683432365169,0.923879532511254,-1.06417654131048E-13));
#23883=DIRECTION('',(0.315985410125162,0.130885442385792,-0.939692620785919));
#23884=DIRECTION('center_axis',(0.382683432365171,-0.923879532511253,1.06417654131048E-13));
#23885=DIRECTION('ref_axis',(-0.923879532511253,-0.382683432365171,4.40796356170094E-14));
#23886=DIRECTION('',(0.923879532511254,0.382683432365169,-4.40796356170092E-14));
#23887=DIRECTION('center_axis',(1.00515054169548E-26,-1.1518563880486E-13,
-1.));
#23888=DIRECTION('ref_axis',(8.72635297355373E-14,-1.,1.1518563880486E-13));
#23889=DIRECTION('',(0.866025403795592,-0.499999999980683,5.75928194002136E-14));
#23890=DIRECTION('',(0.866025403795504,0.499999999980834,-5.75928194002136E-14));
#23891=DIRECTION('',(-8.72635297355373E-14,1.,-1.1518563880486E-13));
#23892=DIRECTION('',(-0.866025403795591,0.499999999980683,-5.75928194002135E-14));
#23893=DIRECTION('',(-0.866025403795504,-0.499999999980834,5.75928194002136E-14));
#23894=DIRECTION('',(8.72635297355373E-14,-1.,1.1518563880486E-13));
#23895=DIRECTION('center_axis',(1.,8.72635297355373E-14,0.));
#23896=DIRECTION('ref_axis',(8.72635297355373E-14,-1.,1.1518563880486E-13));
#23897=DIRECTION('',(4.36317648660808E-14,-0.499999999980658,0.866025403795606));
#23898=DIRECTION('',(-4.36317648660983E-14,0.499999999980858,0.86602540379549));
#23899=DIRECTION('',(-8.72635297355373E-14,1.,-1.1518563880486E-13));
#23900=DIRECTION('',(-4.36317648660808E-14,0.499999999980658,-0.866025403795606));
#23901=DIRECTION('',(4.36317648660983E-14,-0.499999999980858,-0.86602540379549));
#23902=DIRECTION('',(8.72635297355373E-14,-1.,1.1518563880486E-13));
#23903=DIRECTION('center_axis',(1.00515054169548E-26,-1.1518563880486E-13,
-1.));
#23904=DIRECTION('ref_axis',(8.72635297355373E-14,-1.,1.1518563880486E-13));
#23905=DIRECTION('',(1.,8.72635297355373E-14,0.));
#23906=DIRECTION('',(-1.,-8.72635297355373E-14,0.));
#23907=DIRECTION('',(-8.72635297355373E-14,1.,-1.1518563880486E-13));
#23908=DIRECTION('center_axis',(-7.55724335758385E-14,0.86602540379549,
-0.499999999980858));
#23909=DIRECTION('ref_axis',(4.36317648660983E-14,-0.499999999980858,-0.86602540379549));
#23910=DIRECTION('',(-1.,-8.72635297355373E-14,0.));
#23911=DIRECTION('',(-4.36317648660983E-14,0.499999999980859,0.86602540379549));
#23912=DIRECTION('center_axis',(-7.55724335758485E-14,0.866025403795606,
0.499999999980658));
#23913=DIRECTION('ref_axis',(-4.36317648660808E-14,0.499999999980658,-0.866025403795606));
#23914=DIRECTION('',(-1.,-8.72635297355373E-14,0.));
#23915=DIRECTION('',(4.36317648660808E-14,-0.499999999980657,0.866025403795606));
#23916=DIRECTION('center_axis',(-1.00515054169548E-26,1.1518563880486E-13,
1.));
#23917=DIRECTION('ref_axis',(-8.72635297355373E-14,1.,-1.1518563880486E-13));
#23918=DIRECTION('',(-1.,-8.72635297355373E-14,0.));
#23919=DIRECTION('',(8.72635297355373E-14,-1.,1.1518563880486E-13));
#23920=DIRECTION('center_axis',(7.55724335758385E-14,-0.86602540379549,
0.499999999980858));
#23921=DIRECTION('ref_axis',(-4.36317648660983E-14,0.499999999980858,0.86602540379549));
#23922=DIRECTION('',(-1.,-8.72635297355373E-14,0.));
#23923=DIRECTION('',(4.36317648660981E-14,-0.499999999980857,-0.866025403795491));
#23924=DIRECTION('center_axis',(7.55724335758485E-14,-0.866025403795606,
-0.499999999980658));
#23925=DIRECTION('ref_axis',(4.36317648660808E-14,-0.499999999980658,0.866025403795606));
#23926=DIRECTION('',(-4.36317648660809E-14,0.49999999998066,-0.866025403795605));
#23927=DIRECTION('center_axis',(-1.,-8.72635297355374E-14,-1.15648231731787E-15));
#23928=DIRECTION('ref_axis',(-1.15648231732792E-15,1.1518563880486E-13,
1.));
#23929=DIRECTION('',(-8.72635297355373E-14,1.,-1.11716191852906E-13));
#23930=DIRECTION('center_axis',(1.,8.69744091562078E-14,3.23084885458356E-29));
#23931=DIRECTION('ref_axis',(8.69744091562078E-14,-1.,1.15648231731787E-13));
#23932=DIRECTION('',(-1.00515054169548E-26,1.1518563880486E-13,1.));
#23933=DIRECTION('center_axis',(-8.72635297355373E-14,1.,-1.11716191852906E-13));
#23934=DIRECTION('ref_axis',(-6.05512374515239E-29,-1.11716191852906E-13,
-1.));
#23935=DIRECTION('',(8.72635297355373E-14,-1.,1.1518563880486E-13));
#23936=DIRECTION('center_axis',(-8.72635297355373E-14,1.,-1.11716191852906E-13));
#23937=DIRECTION('ref_axis',(-6.05512374515239E-29,-1.11716191852906E-13,
-1.));
#23938=DIRECTION('center_axis',(8.72635297355373E-14,-1.,1.11716191852906E-13));
#23939=DIRECTION('ref_axis',(-6.05512374515239E-29,-1.11716191852906E-13,
-1.));
#23940=DIRECTION('center_axis',(1.00393149750153E-26,-1.1518563880486E-13,
-1.));
#23941=DIRECTION('ref_axis',(-1.,-8.72635297355373E-14,1.219044193949E-29));
#23942=DIRECTION('',(-1.,-8.72635297355373E-14,-1.40416384211369E-42));
#23943=DIRECTION('',(-8.72635297355373E-14,1.,-1.1518563880486E-13));
#23944=DIRECTION('center_axis',(-9.56709551734248E-27,1.09634523681734E-13,
1.));
#23945=DIRECTION('ref_axis',(8.88178419700124E-14,-1.,1.09634523681734E-13));
#23946=DIRECTION('',(1.,8.69608263101991E-14,3.48670874160052E-29));
#23947=DIRECTION('center_axis',(0.866025403784439,1.97253548418658E-14,
-0.5));
#23948=DIRECTION('ref_axis',(-0.5,-1.43385454223916E-13,-0.866025403784439));
#23949=DIRECTION('',(8.57516739673986E-14,-1.,1.14312768470149E-13));
#23950=DIRECTION('',(0.499999999999999,1.43385454223916E-13,0.866025403784439));
#23951=DIRECTION('',(-8.72635297355373E-14,1.,-1.1518563880486E-13));
#23952=DIRECTION('center_axis',(1.00393149750153E-26,-1.1518563880486E-13,
-1.));
#23953=DIRECTION('ref_axis',(-1.,-8.72635297355373E-14,1.219044193949E-29));
#23954=DIRECTION('',(1.,8.72635297355373E-14,1.40416384211369E-42));
#23955=DIRECTION('',(-8.57516739673986E-14,1.,-1.14312768470149E-13));
#23956=DIRECTION('center_axis',(-0.866025403784439,-1.31419512307882E-13,
-0.5));
#23957=DIRECTION('ref_axis',(-0.5,5.61219244883788E-14,0.866025403784439));
#23958=DIRECTION('',(0.5,-5.61219244883788E-14,-0.866025403784439));
#23959=DIRECTION('',(-8.8775385503676E-14,1.,-1.14312768470149E-13));
#23960=DIRECTION('center_axis',(-0.866025403784438,-1.97253548418655E-14,
0.5));
#23961=DIRECTION('ref_axis',(0.5,1.43385454223916E-13,0.866025403784438));
#23962=DIRECTION('',(-0.499999999999999,-1.43385454223916E-13,-0.866025403784439));
#23963=DIRECTION('',(-8.72635297355373E-14,1.,-1.11694157466017E-13));
#23964=DIRECTION('center_axis',(1.20185167897997E-15,1.11694157466017E-13,
1.));
#23965=DIRECTION('ref_axis',(-8.72635297355373E-14,1.,-1.11694157466017E-13));
#23966=DIRECTION('',(-1.,-8.72635297355373E-14,-1.40416384211369E-42));
#23967=DIRECTION('',(-8.57516739673986E-14,1.,-1.14312768470149E-13));
#23968=DIRECTION('center_axis',(0.866025403784439,1.31419512307882E-13,
0.5));
#23969=DIRECTION('ref_axis',(0.5,-5.61219244883789E-14,-0.866025403784439));
#23970=DIRECTION('',(-0.499999999999983,5.61219244883814E-14,0.866025403784448));
#23971=DIRECTION('center_axis',(-8.72635297355373E-14,1.,-1.11716191852906E-13));
#23972=DIRECTION('ref_axis',(-6.05512374515382E-29,-1.11716191852906E-13,
-1.));
#23973=DIRECTION('',(8.72635297355373E-14,-1.,1.1518563880486E-13));
#23974=DIRECTION('center_axis',(-8.72635297355373E-14,1.,-1.11716191852906E-13));
#23975=DIRECTION('ref_axis',(-6.05512374515382E-29,-1.11716191852906E-13,
-1.));
#23976=DIRECTION('',(-8.72635297355373E-14,1.,-1.11694157466017E-13));
#23977=DIRECTION('center_axis',(-8.72635297355373E-14,1.,-1.11716191852906E-13));
#23978=DIRECTION('ref_axis',(-6.05512374515382E-29,-1.11716191852906E-13,
-1.));
#23979=DIRECTION('center_axis',(-9.74682643132153E-27,1.11694157466017E-13,
1.));
#23980=DIRECTION('ref_axis',(-8.72635297355373E-14,1.,-1.11694157466017E-13));
#23981=DIRECTION('',(-1.,-8.69608263101991E-14,-3.48670874160052E-29));
#23982=DIRECTION('center_axis',(9.56709551734248E-27,-1.09634523681734E-13,
-1.));
#23983=DIRECTION('ref_axis',(8.88178419700124E-14,-1.,1.09634523681734E-13));
#23984=DIRECTION('',(8.72635297355373E-14,-1.,1.11694157466017E-13));
#23985=DIRECTION('',(-1.,-8.72635297355373E-14,0.));
#23986=DIRECTION('center_axis',(0.866025403784438,1.97253548418655E-14,
-0.5));
#23987=DIRECTION('ref_axis',(-0.5,-1.43385454223916E-13,-0.866025403784438));
#23988=DIRECTION('',(8.57516739673986E-14,-1.,1.14312768470149E-13));
#23989=DIRECTION('',(-0.499999999999999,-1.40981750865936E-13,-0.866025403784439));
#23990=DIRECTION('',(-8.72635297355373E-14,1.,-1.1518563880486E-13));
#23991=DIRECTION('center_axis',(0.866025403784439,1.31419512307882E-13,
0.5));
#23992=DIRECTION('ref_axis',(0.5,-5.6121924488379E-14,-0.866025403784439));
#23993=DIRECTION('',(8.72635297355373E-14,-1.,1.11694157466017E-13));
#23994=DIRECTION('',(0.499999999999999,-5.37182211303998E-14,-0.866025403784439));
#23995=DIRECTION('center_axis',(-9.74682643132153E-27,1.11694157466017E-13,
1.));
#23996=DIRECTION('ref_axis',(-8.72635297355373E-14,1.,-1.11694157466017E-13));
#23997=DIRECTION('',(8.8775385503676E-14,-1.,1.14312768470149E-13));
#23998=DIRECTION('',(1.,8.72635297355373E-14,0.));
#23999=DIRECTION('center_axis',(-0.866025403784438,-1.97253548418655E-14,
0.5));
#24000=DIRECTION('ref_axis',(0.5,1.43385454223916E-13,0.866025403784438));
#24001=DIRECTION('',(8.57516739673986E-14,-1.,1.14312768470149E-13));
#24002=DIRECTION('',(0.499999999999999,1.40981750865936E-13,0.866025403784439));
#24003=DIRECTION('center_axis',(-0.866025403784439,-1.31419512307882E-13,
-0.5));
#24004=DIRECTION('ref_axis',(-0.5,5.61219244883789E-14,0.866025403784439));
#24005=DIRECTION('',(8.72635297355373E-14,-1.,1.1518563880486E-13));
#24006=DIRECTION('',(-0.499999999999999,5.37182211303996E-14,0.866025403784439));
#24007=DIRECTION('center_axis',(1.00393149750153E-26,-1.1518563880486E-13,
-1.));
#24008=DIRECTION('ref_axis',(-1.,-8.72635297355373E-14,1.219044193949E-29));
#24009=DIRECTION('',(-1.,-8.72635297355373E-14,0.));
#24010=DIRECTION('center_axis',(9.74874922969709E-27,-1.11716191852906E-13,
-1.));
#24011=DIRECTION('ref_axis',(-0.178927238307379,0.983862309163073,-1.09913350487307E-13));
#24012=DIRECTION('',(1.00515054169548E-26,-1.1518563880486E-13,-1.));
#24013=DIRECTION('center_axis',(9.74874922969709E-27,-1.11716191852906E-13,
-1.));
#24014=DIRECTION('ref_axis',(-8.65487012177139E-14,1.,-1.11716191852906E-13));
#24015=DIRECTION('center_axis',(9.74874922969709E-27,-1.11716191852906E-13,
-1.));
#24016=DIRECTION('ref_axis',(-8.61046120078639E-14,1.,-1.11716191852906E-13));
#24017=DIRECTION('center_axis',(-0.866025403784341,-1.24346714277096E-12,
0.50000000000017));
#24018=DIRECTION('ref_axis',(0.50000000000017,5.32565284059118E-10,0.866025403784341));
#24019=DIRECTION('center_axis',(-0.866025403784439,-1.97253548418657E-14,
0.5));
#24020=DIRECTION('ref_axis',(0.5,1.43385454223916E-13,0.866025403784439));
#24021=DIRECTION('',(8.72635297355373E-14,-1.,1.11716191852906E-13));
#24022=DIRECTION('center_axis',(0.866025403784439,2.16945826683511E-14,
-0.5));
#24023=DIRECTION('ref_axis',(0.5,-5.04270596729575E-12,0.866025403784439));
#24024=DIRECTION('',(-0.499999999999999,-1.40981750865936E-13,-0.866025403784439));
#24025=DIRECTION('center_axis',(-8.72635297355373E-14,1.,-1.11716191852906E-13));
#24026=DIRECTION('ref_axis',(6.05512374515455E-29,-1.11716191852906E-13,
-1.));
#24027=DIRECTION('center_axis',(8.72635297355373E-14,-1.,1.11716191852906E-13));
#24028=DIRECTION('ref_axis',(8.67361737988409E-15,-1.11716191852906E-13,
-1.));
#24029=DIRECTION('center_axis',(-8.72635297355373E-14,1.,-1.11694157466017E-13));
#24030=DIRECTION('ref_axis',(9.74682643132155E-27,-1.11694157466017E-13,
-1.));
#24031=DIRECTION('center_axis',(-8.72635297355373E-14,1.,-1.11716191852906E-13));
#24032=DIRECTION('ref_axis',(6.05512374515455E-29,-1.11716191852906E-13,
-1.));
#24033=DIRECTION('',(-1.,-8.69744091562078E-14,-3.22930795142916E-29));
#24034=DIRECTION('',(0.5,-5.61219244883788E-14,-0.866025403784439));
#24035=DIRECTION('center_axis',(-8.72635297355373E-14,1.,-1.11716191852906E-13));
#24036=DIRECTION('ref_axis',(6.05512374515455E-29,-1.11716191852906E-13,
-1.));
#24037=DIRECTION('',(8.57516739673986E-14,-1.,1.14312768470149E-13));
#24038=DIRECTION('center_axis',(0.866025403784439,1.31419512307882E-13,
0.5));
#24039=DIRECTION('ref_axis',(0.5,-5.61219244883788E-14,-0.866025403784439));
#24040=DIRECTION('center_axis',(-0.866025403784486,-5.29905354331503E-14,
-0.499999999999918));
#24041=DIRECTION('ref_axis',(0.499999999999918,-1.6531018130455E-11,-0.866025403784486));
#24042=DIRECTION('center_axis',(9.74874922969709E-27,-1.11716191852906E-13,
-1.));
#24043=DIRECTION('ref_axis',(-8.56605227980138E-14,1.,-1.11716191852906E-13));
#24044=DIRECTION('center_axis',(9.74874922969709E-27,-1.11716191852906E-13,
-1.));
#24045=DIRECTION('ref_axis',(-8.56605227980138E-14,1.,-1.11716191852906E-13));
#24046=DIRECTION('center_axis',(9.74874922969709E-27,-1.11716191852906E-13,
-1.));
#24047=DIRECTION('ref_axis',(0.170744263336185,0.985315379225243,-1.10075681941145E-13));
#24048=DIRECTION('',(-1.00515054169548E-26,1.1518563880486E-13,1.));
#24049=DIRECTION('center_axis',(8.69608263101991E-14,-1.,1.1518563880486E-13));
#24050=DIRECTION('ref_axis',(-1.,-8.69608263101991E-14,-3.48670874160055E-29));
#24051=DIRECTION('',(9.56709551734248E-27,-1.09634523681734E-13,-1.));
#24052=DIRECTION('',(-1.,-8.69744091562078E-14,-3.22930795142916E-29));
#24053=DIRECTION('',(1.,8.69744091562078E-14,3.23084885458356E-29));
#24054=DIRECTION('center_axis',(-1.,-8.72635297355372E-14,1.15648231731787E-15));
#24055=DIRECTION('ref_axis',(1.15648231730782E-15,1.1518563880486E-13,1.));
#24056=DIRECTION('',(9.74682643132155E-27,-1.11694157466017E-13,-1.));
#24057=DIRECTION('center_axis',(1.,8.69744091562078E-14,3.22930795142916E-29));
#24058=DIRECTION('ref_axis',(-8.69744091562078E-14,1.,-1.14491749414469E-13));
#24059=DIRECTION('center_axis',(8.69608263101991E-14,-1.,1.1518563880486E-13));
#24060=DIRECTION('ref_axis',(-1.,-8.69608263101991E-14,-3.48670874160055E-29));
#24061=DIRECTION('',(-1.,-8.72635297355373E-14,0.));
#24062=DIRECTION('',(-9.56709551734248E-27,1.09634523681734E-13,1.));
#24063=DIRECTION('',(1.,8.72635297355373E-14,-1.21904419394898E-29));
#24064=DIRECTION('center_axis',(8.72635297355373E-14,-1.,1.11716191852906E-13));
#24065=DIRECTION('ref_axis',(-6.05512374515239E-29,-1.11716191852906E-13,
-1.));
#24066=DIRECTION('',(1.,8.69744091562078E-14,3.23084885458356E-29));
#24067=DIRECTION('',(-1.,-8.69744091562078E-14,-3.22930795142916E-29));
#24068=DIRECTION('center_axis',(8.72635297355373E-14,-1.,1.11716191852906E-13));
#24069=DIRECTION('ref_axis',(-6.05512374515382E-29,-1.11716191852906E-13,
-1.));
#24070=DIRECTION('center_axis',(1.,8.72635297355372E-14,-1.15648231731787E-15));
#24071=DIRECTION('ref_axis',(-1.15648231730782E-15,-1.1518563880486E-13,
-1.));
#24072=DIRECTION('',(-9.74682643132155E-27,1.11694157466017E-13,1.));
#24073=DIRECTION('center_axis',(-1.,-8.69744091562078E-14,-3.23084885458356E-29));
#24074=DIRECTION('ref_axis',(8.69744091562078E-14,-1.,1.15648231731787E-13));
#24075=DIRECTION('',(8.72635297355373E-14,-1.,1.11716191852906E-13));
#24076=DIRECTION('center_axis',(-8.72635297355373E-14,1.,-1.11716191852906E-13));
#24077=DIRECTION('ref_axis',(-6.05512374515239E-29,-1.11716191852906E-13,
-1.));
#24078=DIRECTION('',(-8.72635297355373E-14,1.,-1.1518563880486E-13));
#24079=DIRECTION('center_axis',(-8.72635297355373E-14,1.,-1.11716191852906E-13));
#24080=DIRECTION('ref_axis',(-6.05512374515239E-29,-1.11716191852906E-13,
-1.));
#24081=DIRECTION('center_axis',(1.00393149750153E-26,-1.1518563880486E-13,
-1.));
#24082=DIRECTION('ref_axis',(-1.,-8.72635297355373E-14,1.219044193949E-29));
#24083=DIRECTION('center_axis',(-9.56709551734248E-27,1.09634523681734E-13,
1.));
#24084=DIRECTION('ref_axis',(8.88178419700124E-14,-1.,1.09634523681734E-13));
#24085=DIRECTION('',(8.72635297355373E-14,-1.,1.1518563880486E-13));
#24086=DIRECTION('',(1.,8.72635297355373E-14,0.));
#24087=DIRECTION('center_axis',(1.,8.69744091562078E-14,3.23084885458356E-29));
#24088=DIRECTION('ref_axis',(8.69744091562078E-14,-1.,1.15648231731787E-13));
#24089=DIRECTION('',(-1.,-8.72635297355373E-14,0.));
#24090=DIRECTION('center_axis',(0.863779089886205,-0.503870701519188,-5.09114224033432E-6));
#24091=DIRECTION('ref_axis',(0.502518782934927,0.861460773419583,0.0732134458752874));
#24092=DIRECTION('',(1.,8.72635297355373E-14,-1.21904419394898E-29));
#24093=DIRECTION('',(1.,8.72635297355373E-14,1.40416384211369E-42));
#24094=DIRECTION('center_axis',(0.866025403784439,1.97253548418657E-14,
-0.5));
#24095=DIRECTION('ref_axis',(-0.5,-1.43385454223916E-13,-0.866025403784439));
#24096=DIRECTION('',(8.57516739673986E-14,-1.,1.14312768470149E-13));
#24097=DIRECTION('',(-0.5,-1.40981750865937E-13,-0.866025403784439));
#24098=DIRECTION('',(-8.72635297355373E-14,1.,-1.1518563880486E-13));
#24099=DIRECTION('center_axis',(0.866025403784439,1.31419512307882E-13,
0.5));
#24100=DIRECTION('ref_axis',(0.5,-5.61219244883788E-14,-0.866025403784439));
#24101=DIRECTION('',(8.72635297355373E-14,-1.,1.11694157466017E-13));
#24102=DIRECTION('',(0.499999999999999,-5.37182211303996E-14,-0.866025403784439));
#24103=DIRECTION('center_axis',(-9.74682643132153E-27,1.11694157466017E-13,
1.));
#24104=DIRECTION('ref_axis',(-8.72635297355373E-14,1.,-1.11694157466017E-13));
#24105=DIRECTION('',(8.87753855036761E-14,-1.,1.14312768470149E-13));
#24106=DIRECTION('',(1.,8.72635297355373E-14,0.));
#24107=DIRECTION('center_axis',(-0.866025403784439,-1.97253548418658E-14,
0.5));
#24108=DIRECTION('ref_axis',(0.5,1.43385454223916E-13,0.866025403784439));
#24109=DIRECTION('',(8.57516739673986E-14,-1.,1.14312768470149E-13));
#24110=DIRECTION('',(0.500000000000008,1.40981750865937E-13,0.866025403784434));
#24111=DIRECTION('center_axis',(-0.866025403784439,-1.31419512307882E-13,
-0.5));
#24112=DIRECTION('ref_axis',(-0.5,5.61219244883789E-14,0.866025403784439));
#24113=DIRECTION('',(8.72635297355373E-14,-1.,1.1518563880486E-13));
#24114=DIRECTION('',(-0.50000000000001,5.37182211303977E-14,0.866025403784433));
#24115=DIRECTION('center_axis',(1.00393149750153E-26,-1.1518563880486E-13,
-1.));
#24116=DIRECTION('ref_axis',(-1.,-8.72635297355373E-14,1.219044193949E-29));
#24117=DIRECTION('',(-1.,-8.72635297355373E-14,0.));
#24118=DIRECTION('center_axis',(1.,8.72635297355374E-14,1.15648231731787E-15));
#24119=DIRECTION('ref_axis',(1.15648231732792E-15,-1.1518563880486E-13,
-1.));
#24120=DIRECTION('',(-8.72635297355373E-14,1.,-1.11716191852906E-13));
#24121=DIRECTION('center_axis',(-1.,-8.69744091562078E-14,-3.22930795142916E-29));
#24122=DIRECTION('ref_axis',(-8.69744091562078E-14,1.,-1.15648231731787E-13));
#24123=DIRECTION('',(1.00515054169548E-26,-1.1518563880486E-13,-1.));
#24124=DIRECTION('center_axis',(-8.72635297355373E-14,1.,-1.11716191852906E-13));
#24125=DIRECTION('ref_axis',(-6.05512374515382E-29,-1.11716191852906E-13,
-1.));
#24126=DIRECTION('',(8.72635297355373E-14,-1.,1.11694157466017E-13));
#24127=DIRECTION('center_axis',(8.72635297355373E-14,-1.,1.11716191852906E-13));
#24128=DIRECTION('ref_axis',(-6.05512374515382E-29,-1.11716191852906E-13,
-1.));
#24129=DIRECTION('center_axis',(-9.74682643132153E-27,1.11694157466017E-13,
1.));
#24130=DIRECTION('ref_axis',(-8.72635297355373E-14,1.,-1.11694157466017E-13));
#24131=DIRECTION('',(1.,8.72635297355373E-14,1.40416384211369E-42));
#24132=DIRECTION('',(-8.72635297355373E-14,1.,-1.11694157466017E-13));
#24133=DIRECTION('center_axis',(9.56709551734248E-27,-1.09634523681734E-13,
-1.));
#24134=DIRECTION('ref_axis',(8.88178419700124E-14,-1.,1.09634523681734E-13));
#24135=DIRECTION('center_axis',(0.866025403784439,1.97253548418658E-14,
-0.5));
#24136=DIRECTION('ref_axis',(-0.5,-1.43385454223916E-13,-0.866025403784439));
#24137=DIRECTION('',(8.57516739673986E-14,-1.,1.14312768470149E-13));
#24138=DIRECTION('',(0.499999999999999,1.43385454223916E-13,0.866025403784439));
#24139=DIRECTION('',(-8.72635297355373E-14,1.,-1.1518563880486E-13));
#24140=DIRECTION('center_axis',(1.00393149750153E-26,-1.1518563880486E-13,
-1.));
#24141=DIRECTION('ref_axis',(-1.,-8.72635297355373E-14,1.219044193949E-29));
#24142=DIRECTION('',(1.,8.72635297355373E-14,1.40416384211369E-42));
#24143=DIRECTION('',(-8.57516739673986E-14,1.,-1.14312768470149E-13));
#24144=DIRECTION('center_axis',(-0.866025403784439,-1.31419512307882E-13,
-0.5));
#24145=DIRECTION('ref_axis',(-0.5,5.61219244883788E-14,0.866025403784439));
#24146=DIRECTION('',(0.500000000000008,-5.61219244883775E-14,-0.866025403784434));
#24147=DIRECTION('',(-8.8775385503676E-14,1.,-1.14312768470149E-13));
#24148=DIRECTION('center_axis',(-0.866025403784438,-1.97253548418655E-14,
0.5));
#24149=DIRECTION('ref_axis',(0.5,1.43385454223916E-13,0.866025403784438));
#24150=DIRECTION('',(-0.500000000000009,-1.43385454223916E-13,-0.866025403784433));
#24151=DIRECTION('',(-8.72635297355373E-14,1.,-1.11694157466017E-13));
#24152=DIRECTION('center_axis',(-9.74682643132153E-27,1.11694157466017E-13,
1.));
#24153=DIRECTION('ref_axis',(-8.72635297355373E-14,1.,-1.11694157466017E-13));
#24154=DIRECTION('',(-1.,-8.72635297355373E-14,-1.40416384211369E-42));
#24155=DIRECTION('',(-8.57516739673986E-14,1.,-1.14312768470149E-13));
#24156=DIRECTION('center_axis',(0.866025403784439,1.31419512307882E-13,
0.5));
#24157=DIRECTION('ref_axis',(0.5,-5.6121924488379E-14,-0.866025403784439));
#24158=DIRECTION('',(-0.499999999999999,5.6121924488379E-14,0.866025403784439));
#24159=DIRECTION('center_axis',(1.00515054169548E-26,-1.1518563880486E-13,
-1.));
#24160=DIRECTION('ref_axis',(8.72635297355373E-14,-1.,1.1518563880486E-13));
#24161=DIRECTION('',(-1.,-8.72635297355373E-14,0.));
#24162=DIRECTION('',(1.,8.72635297355373E-14,0.));
#24163=DIRECTION('',(8.72635297355373E-14,-1.,1.1518563880486E-13));
#24164=DIRECTION('center_axis',(7.55724335758485E-14,-0.866025403795606,
-0.499999999980658));
#24165=DIRECTION('ref_axis',(4.36317648660808E-14,-0.499999999980658,0.866025403795606));
#24166=DIRECTION('',(1.,8.72635297355373E-14,0.));
#24167=DIRECTION('',(4.36317648660808E-14,-0.499999999980658,0.866025403795606));
#24168=DIRECTION('center_axis',(7.55724335758385E-14,-0.86602540379549,
0.499999999980858));
#24169=DIRECTION('ref_axis',(-4.36317648660983E-14,0.499999999980858,0.86602540379549));
#24170=DIRECTION('',(1.,8.72635297355373E-14,0.));
#24171=DIRECTION('',(-4.36317648660983E-14,0.499999999980859,0.86602540379549));
#24172=DIRECTION('center_axis',(-1.00515054169548E-26,1.1518563880486E-13,
1.));
#24173=DIRECTION('ref_axis',(-8.72635297355373E-14,1.,-1.1518563880486E-13));
#24174=DIRECTION('',(1.,8.72635297355373E-14,0.));
#24175=DIRECTION('',(-8.72635297355373E-14,1.,-1.1518563880486E-13));
#24176=DIRECTION('center_axis',(-7.55724335758485E-14,0.866025403795606,
0.499999999980658));
#24177=DIRECTION('ref_axis',(-4.36317648660808E-14,0.499999999980658,-0.866025403795606));
#24178=DIRECTION('',(1.,8.72635297355373E-14,0.));
#24179=DIRECTION('',(-4.36317648660809E-14,0.499999999980659,-0.866025403795605));
#24180=DIRECTION('center_axis',(-7.55724335758385E-14,0.86602540379549,
-0.499999999980858));
#24181=DIRECTION('ref_axis',(4.36317648660983E-14,-0.499999999980858,-0.86602540379549));
#24182=DIRECTION('',(4.36317648660983E-14,-0.499999999980858,-0.86602540379549));
#24183=DIRECTION('center_axis',(-1.00515054169548E-26,1.1518563880486E-13,
1.));
#24184=DIRECTION('ref_axis',(-8.72635297355373E-14,1.,-1.1518563880486E-13));
#24185=DIRECTION('center_axis',(1.,8.72635297355373E-14,0.));
#24186=DIRECTION('ref_axis',(8.72635297355373E-14,-1.,1.1518563880486E-13));
#24187=DIRECTION('',(4.36317648660808E-14,-0.499999999980658,0.866025403795606));
#24188=DIRECTION('',(-4.36317648660983E-14,0.499999999980858,0.86602540379549));
#24189=DIRECTION('',(-8.72635297355373E-14,1.,-1.1518563880486E-13));
#24190=DIRECTION('',(-4.36317648660808E-14,0.499999999980658,-0.866025403795606));
#24191=DIRECTION('',(4.36317648660983E-14,-0.499999999980858,-0.86602540379549));
#24192=DIRECTION('',(8.72635297355373E-14,-1.,1.1518563880486E-13));
#24193=DIRECTION('center_axis',(-1.00515054169548E-26,1.1518563880486E-13,
1.));
#24194=DIRECTION('ref_axis',(-8.72635297355373E-14,1.,-1.1518563880486E-13));
#24195=DIRECTION('center_axis',(1.00515054169548E-26,-1.1518563880486E-13,
-1.));
#24196=DIRECTION('ref_axis',(8.72635297355373E-14,-1.,1.1518563880486E-13));
#24197=DIRECTION('',(-1.,-8.72635297355373E-14,0.));
#24198=DIRECTION('',(-0.206879256138141,0.978366482142418,-1.1269376823084E-13));
#24199=DIRECTION('',(0.238241565688704,-0.971205928924548,1.11868975334244E-13));
#24200=DIRECTION('',(1.,8.72635297355373E-14,0.));
#24201=DIRECTION('',(0.238241565688535,0.97120592892459,-1.11868975334244E-13));
#24202=DIRECTION('',(-0.20687925613797,-0.978366482142454,1.1269376823084E-13));
#24203=DIRECTION('center_axis',(-8.72635297355373E-14,1.,-1.1518563880486E-13));
#24204=DIRECTION('ref_axis',(1.00515054169548E-26,-1.1518563880486E-13,
-1.));
#24205=DIRECTION('',(1.,8.72635297355373E-14,0.));
#24206=DIRECTION('',(-1.00515054169548E-26,1.1518563880486E-13,1.));
#24207=DIRECTION('',(1.00515054169548E-26,-1.1518563880486E-13,-1.));
#24208=DIRECTION('center_axis',(1.00515054169548E-26,-1.1518563880486E-13,
-1.));
#24209=DIRECTION('ref_axis',(8.72635297355373E-14,-1.,1.1518563880486E-13));
#24210=DIRECTION('',(0.206879256138141,-0.978366482142418,1.1269376823084E-13));
#24211=DIRECTION('',(0.20687925613797,0.978366482142454,-1.1269376823084E-13));
#24212=DIRECTION('',(-0.238241565688535,-0.97120592892459,1.11868975334244E-13));
#24213=DIRECTION('',(-1.,-8.72635297355373E-14,0.));
#24214=DIRECTION('',(-0.238241565688704,0.971205928924548,-1.11868975334244E-13));
#24215=DIRECTION('center_axis',(-8.72635297355373E-14,1.,-1.1518563880486E-13));
#24216=DIRECTION('ref_axis',(1.00515054169548E-26,-1.1518563880486E-13,
-1.));
#24217=DIRECTION('',(1.,8.72635297355373E-14,0.));
#24218=DIRECTION('',(-1.00515054169548E-26,1.1518563880486E-13,1.));
#24219=DIRECTION('',(1.00515054169548E-26,-1.1518563880486E-13,-1.));
#24220=DIRECTION('center_axis',(-1.,-8.72635297355373E-14,0.));
#24221=DIRECTION('ref_axis',(-8.72635297355373E-14,1.,-1.1518563880486E-13));
#24222=DIRECTION('',(1.00515054169548E-26,-1.1518563880486E-13,-1.));
#24223=DIRECTION('',(-1.00515054169548E-26,1.1518563880486E-13,1.));
#24224=DIRECTION('',(-8.72635297355373E-14,1.,-1.1518563880486E-13));
#24225=DIRECTION('center_axis',(-0.499999999980834,0.866025403795504,-9.9753689357427E-14));
#24226=DIRECTION('ref_axis',(0.866025403795504,0.499999999980834,-5.75928194002136E-14));
#24227=DIRECTION('',(-1.00515054169548E-26,1.1518563880486E-13,1.));
#24228=DIRECTION('',(0.866025403795504,0.499999999980834,-5.75928194002136E-14));
#24229=DIRECTION('center_axis',(0.499999999980683,0.866025403795592,-9.9753689357427E-14));
#24230=DIRECTION('ref_axis',(0.866025403795591,-0.499999999980683,5.75928194002136E-14));
#24231=DIRECTION('',(-1.00515054169548E-26,1.1518563880486E-13,1.));
#24232=DIRECTION('',(0.866025403795592,-0.499999999980682,5.75928194002136E-14));
#24233=DIRECTION('center_axis',(1.,8.72635297355373E-14,0.));
#24234=DIRECTION('ref_axis',(8.72635297355373E-14,-1.,1.1518563880486E-13));
#24235=DIRECTION('',(-1.00515054169548E-26,1.1518563880486E-13,1.));
#24236=DIRECTION('',(8.72635297355373E-14,-1.,1.1518563880486E-13));
#24237=DIRECTION('center_axis',(0.499999999980834,-0.866025403795504,9.9753689357427E-14));
#24238=DIRECTION('ref_axis',(-0.866025403795504,-0.499999999980834,5.75928194002136E-14));
#24239=DIRECTION('',(-1.00515054169548E-26,1.1518563880486E-13,1.));
#24240=DIRECTION('',(-0.866025403795505,-0.499999999980833,5.75928194002135E-14));
#24241=DIRECTION('center_axis',(-0.499999999980683,-0.866025403795592,9.9753689357427E-14));
#24242=DIRECTION('ref_axis',(-0.866025403795591,0.499999999980683,-5.75928194002136E-14));
#24243=DIRECTION('',(-0.866025403795592,0.499999999980682,-5.75928194002135E-14));
#24244=DIRECTION('center_axis',(1.00515054169548E-26,-1.1518563880486E-13,
-1.));
#24245=DIRECTION('ref_axis',(8.72635297355373E-14,-1.,1.1518563880486E-13));
#24246=DIRECTION('center_axis',(1.00515054169548E-26,-1.1518563880486E-13,
-1.));
#24247=DIRECTION('ref_axis',(8.67361737988404E-14,-1.,1.1518563880486E-13));
#24248=DIRECTION('',(-8.72635297355373E-14,1.,-1.1518563880486E-13));
#24249=DIRECTION('',(1.,8.72635297355373E-14,0.));
#24250=DIRECTION('',(-1.,-8.72635297355373E-14,0.));
#24251=DIRECTION('',(-8.72635297355373E-14,1.,-1.1518563880486E-13));
#24252=DIRECTION('center_axis',(-7.55724335758385E-14,0.86602540379549,
-0.499999999980858));
#24253=DIRECTION('ref_axis',(4.36317648660983E-14,-0.499999999980858,-0.86602540379549));
#24254=DIRECTION('',(-1.,-8.72635297355373E-14,0.));
#24255=DIRECTION('',(-4.36317648660983E-14,0.499999999980858,0.86602540379549));
#24256=DIRECTION('center_axis',(-7.55724335758485E-14,0.866025403795606,
0.499999999980658));
#24257=DIRECTION('ref_axis',(-4.36317648660808E-14,0.499999999980658,-0.866025403795606));
#24258=DIRECTION('',(-1.,-8.72635297355373E-14,0.));
#24259=DIRECTION('',(4.36317648660809E-14,-0.499999999980659,0.866025403795605));
#24260=DIRECTION('center_axis',(-1.00515054169548E-26,1.1518563880486E-13,
1.));
#24261=DIRECTION('ref_axis',(-8.72635297355373E-14,1.,-1.1518563880486E-13));
#24262=DIRECTION('',(-1.,-8.72635297355373E-14,0.));
#24263=DIRECTION('',(8.72635297355373E-14,-1.,1.1518563880486E-13));
#24264=DIRECTION('center_axis',(-1.00515054169548E-26,1.1518563880486E-13,
1.));
#24265=DIRECTION('ref_axis',(1.11022302462516E-13,-1.,1.1518563880486E-13));
#24266=DIRECTION('',(8.72635297355373E-14,-1.,1.1518563880486E-13));
#24267=DIRECTION('center_axis',(7.55724335758385E-14,-0.86602540379549,
0.499999999980858));
#24268=DIRECTION('ref_axis',(-4.36317648660983E-14,0.499999999980858,0.86602540379549));
#24269=DIRECTION('',(-1.,-8.72635297355373E-14,0.));
#24270=DIRECTION('',(4.36317648660983E-14,-0.499999999980859,-0.86602540379549));
#24271=DIRECTION('center_axis',(7.55724335758485E-14,-0.866025403795606,
-0.499999999980658));
#24272=DIRECTION('ref_axis',(4.36317648660808E-14,-0.499999999980658,0.866025403795606));
#24273=DIRECTION('',(-4.36317648660808E-14,0.499999999980658,-0.866025403795606));
#24274=DIRECTION('center_axis',(-1.,-8.72635297355373E-14,0.));
#24275=DIRECTION('ref_axis',(-8.72635297355373E-14,1.,-1.1518563880486E-13));
#24276=DIRECTION('center_axis',(9.56709551734248E-27,-1.09634523681734E-13,
-1.));
#24277=DIRECTION('ref_axis',(8.88178419700124E-14,-1.,1.09634523681734E-13));
#24278=DIRECTION('',(-1.00572058919142E-26,1.1518563880486E-13,1.));
#24279=DIRECTION('center_axis',(8.72635297355373E-14,-1.,1.1518563880486E-13));
#24280=DIRECTION('ref_axis',(-1.,-8.72635297355373E-14,-1.43492962746861E-42));
#24281=DIRECTION('center_axis',(8.89982532115141E-14,-1.,1.11694157466017E-13));
#24282=DIRECTION('ref_axis',(9.25185853854302E-15,-1.11694157466016E-13,
-1.));
#24283=DIRECTION('',(-1.00572058919142E-26,1.1518563880486E-13,1.));
#24284=DIRECTION('center_axis',(0.863769935395407,0.503886382132179,0.000112288726983334));
#24285=DIRECTION('ref_axis',(0.502538534396613,-0.861475679507312,0.0729018179740325));
#24286=DIRECTION('center_axis',(-8.72635297355373E-14,1.,-1.11694157466017E-13));
#24287=DIRECTION('ref_axis',(9.74682643132155E-27,-1.11694157466017E-13,
-1.));
#24288=DIRECTION('',(-1.,-8.69744091562078E-14,-3.22930795142916E-29));
#24289=DIRECTION('',(-1.00572058919142E-26,1.1518563880486E-13,1.));
#24290=DIRECTION('center_axis',(8.89982532115141E-14,-1.,1.11694157466017E-13));
#24291=DIRECTION('ref_axis',(-5.97939217230155E-29,1.11694157466017E-13,
1.));
#24292=DIRECTION('center_axis',(-1.,-8.69744091562078E-14,-3.22930795142916E-29));
#24293=DIRECTION('ref_axis',(-8.69744091562078E-14,1.,-1.15648231731787E-13));
#24294=DIRECTION('',(1.,8.72635297355373E-14,-1.21904419394898E-29));
#24295=DIRECTION('center_axis',(0.863777735208662,-0.503873023735671,-1.04530852487832E-5));
#24296=DIRECTION('ref_axis',(0.502519089939509,0.861458237603484,-0.0732411708772271));
#24297=DIRECTION('',(-1.,-8.72635297355373E-14,-1.40416384211369E-42));
#24298=DIRECTION('center_axis',(1.00515054169548E-26,-1.1518563880486E-13,
-1.));
#24299=DIRECTION('ref_axis',(8.72635297355373E-14,-1.,1.1518563880486E-13));
#24300=DIRECTION('',(0.238241565688704,-0.971205928924548,1.11868975334244E-13));
#24301=DIRECTION('',(0.238241565688534,0.97120592892459,-1.11868975334244E-13));
#24302=DIRECTION('',(-1.,-8.72635297355373E-14,0.));
#24303=DIRECTION('center_axis',(-8.89982532115141E-14,1.,-1.11694157466017E-13));
#24304=DIRECTION('ref_axis',(5.9793921723027E-29,-1.11694157466017E-13,
-1.));
#24305=DIRECTION('center_axis',(8.89982532115141E-14,-1.,1.11694157466017E-13));
#24306=DIRECTION('ref_axis',(-4.31309843882671E-29,-1.11694157466017E-13,
-1.));
#24307=DIRECTION('',(-8.88962106541037E-14,1.,-1.1518563880486E-13));
#24308=DIRECTION('',(-8.72635297355373E-14,1.,-1.1518563880486E-13));
#24309=DIRECTION('center_axis',(1.00393149750153E-26,-1.1518563880486E-13,
-1.));
#24310=DIRECTION('ref_axis',(-1.,-8.72635297355373E-14,1.219044193949E-29));
#24311=DIRECTION('',(1.,8.72635297355373E-14,0.));
#24312=DIRECTION('',(-8.55288062595605E-14,1.,-1.11694157466017E-13));
#24313=DIRECTION('center_axis',(9.56709551734248E-27,-1.09634523681734E-13,
-1.));
#24314=DIRECTION('ref_axis',(8.88178419700124E-14,-1.,1.09634523681734E-13));
#24315=DIRECTION('',(1.00484705889771E-26,-1.1518563880486E-13,-1.));
#24316=DIRECTION('center_axis',(-8.72635297355373E-14,1.,-1.11694157466017E-13));
#24317=DIRECTION('ref_axis',(9.74682643132155E-27,-1.11694157466017E-13,
-1.));
#24318=DIRECTION('',(1.00484705889771E-26,-1.1518563880486E-13,-1.));
#24319=DIRECTION('center_axis',(8.55288062595605E-14,-1.,1.11694157466017E-13));
#24320=DIRECTION('ref_axis',(-5.74629564289751E-29,1.11694157466017E-13,
1.));
#24321=DIRECTION('center_axis',(8.55288062595605E-14,-1.,1.11694157466017E-13));
#24322=DIRECTION('ref_axis',(-5.74629564289751E-29,1.11694157466017E-13,
1.));
#24323=DIRECTION('center_axis',(8.55288062595605E-14,-1.,1.11694157466017E-13));
#24324=DIRECTION('ref_axis',(4.14495956315118E-29,1.11694157466017E-13,
1.));
#24325=DIRECTION('',(8.72635297355373E-14,-1.,1.1518563880486E-13));
#24326=DIRECTION('center_axis',(8.72635297355373E-14,-1.,1.1518563880486E-13));
#24327=DIRECTION('ref_axis',(-1.,-8.72635297355373E-14,-1.43492962746861E-42));
#24328=DIRECTION('center_axis',(8.56308488169709E-14,-1.,1.11694157466017E-13));
#24329=DIRECTION('ref_axis',(5.75315142317297E-29,-1.11694157466017E-13,
-1.));
#24330=DIRECTION('',(1.00484705889771E-26,-1.1518563880486E-13,-1.));
#24331=DIRECTION('center_axis',(1.,8.72635297355373E-14,0.));
#24332=DIRECTION('ref_axis',(8.72635297355373E-14,-1.,1.1518563880486E-13));
#24333=DIRECTION('center_axis',(1.00515054169548E-26,-1.1518563880486E-13,
-1.));
#24334=DIRECTION('ref_axis',(8.72635297355373E-14,-1.,1.1518563880486E-13));
#24335=DIRECTION('',(1.,8.72635297355373E-14,0.));
#24336=DIRECTION('',(-1.,-8.72635297355373E-14,0.));
#24337=DIRECTION('',(-8.72635297355373E-14,1.,-1.1518563880486E-13));
#24338=DIRECTION('center_axis',(-7.55724335758385E-14,0.86602540379549,
-0.499999999980858));
#24339=DIRECTION('ref_axis',(4.36317648660983E-14,-0.499999999980858,-0.86602540379549));
#24340=DIRECTION('',(-1.,-8.72635297355373E-14,0.));
#24341=DIRECTION('',(-4.36317648660978E-14,0.499999999980852,0.866025403795494));
#24342=DIRECTION('center_axis',(-7.55724335758485E-14,0.866025403795606,
0.499999999980658));
#24343=DIRECTION('ref_axis',(-4.36317648660808E-14,0.499999999980658,-0.866025403795606));
#24344=DIRECTION('',(-1.,-8.72635297355373E-14,0.));
#24345=DIRECTION('',(4.36317648660803E-14,-0.499999999980653,0.866025403795609));
#24346=DIRECTION('center_axis',(-1.00515054169548E-26,1.1518563880486E-13,
1.));
#24347=DIRECTION('ref_axis',(-8.72635297355373E-14,1.,-1.1518563880486E-13));
#24348=DIRECTION('',(-1.,-8.72635297355373E-14,0.));
#24349=DIRECTION('',(8.72635297355373E-14,-1.,1.1518563880486E-13));
#24350=DIRECTION('center_axis',(7.55724335758385E-14,-0.86602540379549,
0.499999999980858));
#24351=DIRECTION('ref_axis',(-4.36317648660983E-14,0.499999999980858,0.86602540379549));
#24352=DIRECTION('',(-1.,-8.72635297355373E-14,0.));
#24353=DIRECTION('',(4.36317648660981E-14,-0.499999999980856,-0.866025403795491));
#24354=DIRECTION('center_axis',(7.55724335758485E-14,-0.866025403795606,
-0.499999999980658));
#24355=DIRECTION('ref_axis',(4.36317648660808E-14,-0.499999999980658,0.866025403795606));
#24356=DIRECTION('',(-4.36317648660806E-14,0.499999999980657,-0.866025403795607));
#24357=DIRECTION('center_axis',(-0.97120592892459,0.238241565688534,-2.74420069337136E-14));
#24358=DIRECTION('ref_axis',(0.238241565688534,0.97120592892459,-1.11868975334244E-13));
#24359=DIRECTION('',(1.00515054169548E-26,-1.1518563880486E-13,-1.));
#24360=DIRECTION('center_axis',(-0.978366482142454,0.20687925613797,-2.38295192737362E-14));
#24361=DIRECTION('ref_axis',(0.20687925613797,0.978366482142454,-1.1269376823084E-13));
#24362=DIRECTION('',(1.00515054169548E-26,-1.1518563880486E-13,-1.));
#24363=DIRECTION('center_axis',(-0.97120592892459,0.238241565688534,-2.74420069337136E-14));
#24364=DIRECTION('ref_axis',(0.238241565688534,0.97120592892459,-1.11868975334244E-13));
#24365=DIRECTION('',(0.238241565688534,0.97120592892459,-1.11868975334244E-13));
#24366=DIRECTION('',(1.00515054169548E-26,-1.1518563880486E-13,-1.));
#24367=DIRECTION('',(-1.00515054169548E-26,1.1518563880486E-13,1.));
#24368=DIRECTION('center_axis',(-8.72635297355373E-14,1.,-1.1518563880486E-13));
#24369=DIRECTION('ref_axis',(1.00515054169548E-26,-1.1518563880486E-13,
-1.));
#24370=DIRECTION('',(1.,8.72635297355373E-14,0.));
#24371=DIRECTION('',(-1.00515054169548E-26,1.1518563880486E-13,1.));
#24372=DIRECTION('center_axis',(0.971205928924548,0.238241565688704,-2.74420069337136E-14));
#24373=DIRECTION('ref_axis',(0.238241565688704,-0.971205928924548,1.11868975334244E-13));
#24374=DIRECTION('',(0.238241565688704,-0.971205928924548,1.11868975334244E-13));
#24375=DIRECTION('',(-1.00515054169548E-26,1.1518563880486E-13,1.));
#24376=DIRECTION('center_axis',(0.978366482142418,0.206879256138141,-2.38295192737362E-14));
#24377=DIRECTION('ref_axis',(0.206879256138141,-0.978366482142418,1.1269376823084E-13));
#24378=DIRECTION('',(-1.00515054169548E-26,1.1518563880486E-13,1.));
#24379=DIRECTION('center_axis',(0.971205928924548,0.238241565688704,-2.74420069337136E-14));
#24380=DIRECTION('ref_axis',(0.238241565688704,-0.971205928924548,1.11868975334244E-13));
#24381=DIRECTION('',(-1.00515054169548E-26,1.1518563880486E-13,1.));
#24382=DIRECTION('center_axis',(-1.00515054169548E-26,1.1518563880486E-13,
1.));
#24383=DIRECTION('ref_axis',(-8.72635297355373E-14,1.,-1.1518563880486E-13));
#24384=DIRECTION('center_axis',(1.,8.72635297355373E-14,0.));
#24385=DIRECTION('ref_axis',(8.72635297355373E-14,-1.,1.1518563880486E-13));
#24386=DIRECTION('',(1.00515054169548E-26,-1.1518563880486E-13,-1.));
#24387=DIRECTION('center_axis',(-1.,-8.72635297355373E-14,0.));
#24388=DIRECTION('ref_axis',(-8.72635297355373E-14,1.,-1.1518563880486E-13));
#24389=DIRECTION('',(1.00515054169548E-26,-1.1518563880486E-13,-1.));
#24390=DIRECTION('',(1.00515054169548E-26,-1.1518563880486E-13,-1.));
#24391=DIRECTION('center_axis',(1.00515054169548E-26,-1.1518563880486E-13,
-1.));
#24392=DIRECTION('ref_axis',(8.72635297355373E-14,-1.,1.1518563880486E-13));
#24393=DIRECTION('',(-8.72635297355373E-14,1.,-1.1518563880486E-13));
#24394=DIRECTION('center_axis',(-1.00515054169548E-26,1.1518563880486E-13,
1.));
#24395=DIRECTION('ref_axis',(8.67361737988404E-14,-1.,1.1518563880486E-13));
#24396=DIRECTION('center_axis',(1.00515054169548E-26,-1.1518563880486E-13,
-1.));
#24397=DIRECTION('ref_axis',(8.72635297355373E-14,-1.,1.1518563880486E-13));
#24398=DIRECTION('',(-8.72635297355373E-14,1.,-1.1518563880486E-13));
#24399=DIRECTION('center_axis',(-1.00515054169548E-26,1.1518563880486E-13,
1.));
#24400=DIRECTION('ref_axis',(8.67361737988403E-14,-1.,1.1518563880486E-13));
#24401=DIRECTION('center_axis',(1.,8.72635297355373E-14,0.));
#24402=DIRECTION('ref_axis',(8.72635297355373E-14,-1.,1.1518563880486E-13));
#24403=DIRECTION('',(-1.00515054169548E-26,1.1518563880486E-13,1.));
#24404=DIRECTION('center_axis',(1.,8.88962106541037E-14,-1.82360919610117E-28));
#24405=DIRECTION('ref_axis',(8.88962106541037E-14,-1.,1.1518563880486E-13));
#24406=DIRECTION('',(1.00515054169548E-26,-1.1518563880486E-13,-1.));
#24407=DIRECTION('',(8.89982532115141E-14,-1.,1.11694157466017E-13));
#24408=DIRECTION('center_axis',(8.89982532115141E-14,-1.,1.11694157466017E-13));
#24409=DIRECTION('ref_axis',(-5.97939217230155E-29,1.11694157466017E-13,
1.));
#24410=DIRECTION('center_axis',(-8.89982532115141E-14,1.,-1.11694157466017E-13));
#24411=DIRECTION('ref_axis',(-2.77555756156289E-14,1.11694157466014E-13,
1.));
#24412=DIRECTION('',(-8.72635297355373E-14,1.,-1.1518563880486E-13));
#24413=DIRECTION('center_axis',(8.89982532115141E-14,-1.,1.11694157466017E-13));
#24414=DIRECTION('ref_axis',(4.31309843882786E-29,1.11694157466017E-13,
1.));
#24415=DIRECTION('center_axis',(1.00393149750153E-26,-1.1518563880486E-13,
-1.));
#24416=DIRECTION('ref_axis',(-1.,-8.72635297355373E-14,1.219044193949E-29));
#24417=DIRECTION('',(8.56308488169709E-14,-1.,1.11694157466017E-13));
#24418=DIRECTION('',(1.,8.69573680357505E-14,3.41964731060544E-29));
#24419=DIRECTION('center_axis',(-8.56308488169709E-14,1.,-1.11694157466017E-13));
#24420=DIRECTION('ref_axis',(-4.14990482420177E-29,-1.11694157466017E-13,
-1.));
#24421=DIRECTION('center_axis',(8.56308488169709E-14,-1.,1.11694157466017E-13));
#24422=DIRECTION('ref_axis',(-4.14990482420177E-29,-1.11694157466017E-13,
-1.));
#24423=DIRECTION('',(-8.72635297355373E-14,1.,-1.1518563880486E-13));
#24424=DIRECTION('center_axis',(-8.56308488169709E-14,1.,-1.11694157466017E-13));
#24425=DIRECTION('ref_axis',(-4.14990482420177E-29,-1.11694157466017E-13,
-1.));
#24426=DIRECTION('center_axis',(-8.72635297355373E-14,1.,-1.1518563880486E-13));
#24427=DIRECTION('ref_axis',(1.00515054169548E-26,-1.1518563880486E-13,
-1.));
#24428=DIRECTION('',(-1.00515054169548E-26,1.1518563880486E-13,1.));
#24429=DIRECTION('',(1.00515054169548E-26,-1.1518563880486E-13,-1.));
#24430=DIRECTION('center_axis',(-1.,-8.72635297355373E-14,3.03482797761984E-30));
#24431=DIRECTION('ref_axis',(-1.00484705889771E-26,1.1518563880486E-13,
1.));
#24432=DIRECTION('',(-1.00515054169548E-26,1.1518563880486E-13,1.));
#24433=DIRECTION('center_axis',(1.00515054169548E-26,-1.1518563880486E-13,
-1.));
#24434=DIRECTION('ref_axis',(8.72635297355373E-14,-1.,1.1518563880486E-13));
#24435=DIRECTION('',(8.72635297355373E-14,-1.,1.1518563880486E-13));
#24436=DIRECTION('center_axis',(-1.00515054169548E-26,1.1518563880486E-13,
1.));
#24437=DIRECTION('ref_axis',(8.90491384334761E-14,-1.,1.1518563880486E-13));
#24438=DIRECTION('center_axis',(1.00515054169548E-26,-1.1518563880486E-13,
-1.));
#24439=DIRECTION('ref_axis',(8.72635297355373E-14,-1.,1.1518563880486E-13));
#24440=DIRECTION('',(8.72635297355373E-14,-1.,1.1518563880486E-13));
#24441=DIRECTION('center_axis',(-1.00515054169548E-26,1.1518563880486E-13,
1.));
#24442=DIRECTION('ref_axis',(8.67361737988404E-14,-1.,1.1518563880486E-13));
#24443=DIRECTION('center_axis',(-1.00515054169548E-26,1.1518563880486E-13,
1.));
#24444=DIRECTION('ref_axis',(-8.72635297355373E-14,1.,-1.1518563880486E-13));
#24445=DIRECTION('center_axis',(-1.00515054169548E-26,1.1518563880486E-13,
1.));
#24446=DIRECTION('ref_axis',(-1.25899290992493E-13,-1.,1.1518563880486E-13));
#24447=DIRECTION('center_axis',(-1.00515054169548E-26,1.1518563880486E-13,
1.));
#24448=DIRECTION('ref_axis',(8.63130705120167E-14,-1.,1.1518563880486E-13));
#24449=DIRECTION('center_axis',(1.00515054169548E-26,-1.1518563880486E-13,
-1.));
#24450=DIRECTION('ref_axis',(-0.46275581060595,0.886485792187574,-1.02110432264563E-13));
#24451=DIRECTION('center_axis',(-1.00515054169548E-26,1.1518563880486E-13,
1.));
#24452=DIRECTION('ref_axis',(8.56289034950253E-14,-1.,1.1518563880486E-13));
#24453=DIRECTION('center_axis',(-1.00515054169548E-26,1.1518563880486E-13,
1.));
#24454=DIRECTION('ref_axis',(8.65147197380774E-14,-1.,1.1518563880486E-13));
#24455=DIRECTION('center_axis',(1.00515054169548E-26,-1.1518563880486E-13,
-1.));
#24456=DIRECTION('ref_axis',(8.72635297355373E-14,-1.,1.1518563880486E-13));
#24457=DIRECTION('center_axis',(1.00515054169548E-26,-1.1518563880486E-13,
-1.));
#24458=DIRECTION('ref_axis',(8.72912853111529E-14,-1.,1.1518563880486E-13));
#24459=DIRECTION('center_axis',(1.00515054169548E-26,-1.1518563880486E-13,
-1.));
#24460=DIRECTION('ref_axis',(8.72635297355373E-14,-1.,1.1518563880486E-13));
#24461=DIRECTION('center_axis',(1.00515054169548E-26,-1.1518563880486E-13,
-1.));
#24462=DIRECTION('ref_axis',(8.72912853111529E-14,-1.,1.1518563880486E-13));
#24463=DIRECTION('center_axis',(1.00515054169548E-26,-1.1518563880486E-13,
-1.));
#24464=DIRECTION('ref_axis',(8.72635297355373E-14,-1.,1.1518563880486E-13));
#24465=DIRECTION('center_axis',(1.00515054169548E-26,-1.1518563880486E-13,
-1.));
#24466=DIRECTION('ref_axis',(8.73285184003934E-14,-1.,1.1518563880486E-13));
#24467=DIRECTION('center_axis',(1.00515054169548E-26,-1.1518563880486E-13,
-1.));
#24468=DIRECTION('ref_axis',(0.232483687494752,0.972600295624488,-1.120295863533E-13));
#24469=DIRECTION('center_axis',(-1.00515054169548E-26,1.1518563880486E-13,
1.));
#24470=DIRECTION('ref_axis',(-8.72635297355373E-14,1.,-1.1518563880486E-13));
#24471=DIRECTION('center_axis',(-1.00515054169548E-26,1.1518563880486E-13,
1.));
#24472=DIRECTION('ref_axis',(8.72425792474809E-14,-1.,1.1518563880486E-13));
#24473=DIRECTION('center_axis',(-1.,-8.72635297355373E-14,0.));
#24474=DIRECTION('ref_axis',(-8.72635297355373E-14,1.,-1.1518563880486E-13));
#24475=DIRECTION('center_axis',(1.00515054169548E-26,-1.1518563880486E-13,
-1.));
#24476=DIRECTION('ref_axis',(8.72635297355373E-14,-1.,1.1518563880486E-13));
#24477=DIRECTION('',(8.72635297355373E-14,-1.,1.1518563880486E-13));
#24478=DIRECTION('',(-0.133254699246628,-0.991081825647454,1.14158393195087E-13));
#24479=DIRECTION('',(0.181426836203858,0.983404445335213,-1.13274069239474E-13));
#24480=DIRECTION('',(-0.148350608954417,0.988934829411349,-1.13911090062123E-13));
#24481=DIRECTION('',(-0.499999999998003,-0.866025403785592,9.97536893562752E-14));
#24482=DIRECTION('',(-1.,-8.72635297355373E-14,0.));
#24483=DIRECTION('center_axis',(-0.983404445335213,0.181426836203859,-2.0897766024496E-14));
#24484=DIRECTION('ref_axis',(0.181426836203859,0.983404445335213,-1.13274069239474E-13));
#24485=DIRECTION('',(-0.181426836203858,-0.983404445335213,1.13274069239474E-13));
#24486=DIRECTION('',(1.00515054169548E-26,-1.1518563880486E-13,-1.));
#24487=DIRECTION('center_axis',(1.00515054169548E-26,-1.1518563880486E-13,
-1.));
#24488=DIRECTION('ref_axis',(8.72635297355373E-14,-1.,1.1518563880486E-13));
#24489=DIRECTION('',(0.189038743476621,0.981969629604083,-1.13108799072916E-13));
#24490=DIRECTION('',(-0.177165010652742,0.984181161677267,-1.13363535807507E-13));
#24491=DIRECTION('',(0.148350608954417,-0.988934829411349,1.13911090062123E-13));
#24492=DIRECTION('center_axis',(-0.981969629604083,0.189038743476621,-2.17745484262326E-14));
#24493=DIRECTION('ref_axis',(0.189038743476621,0.981969629604083,-1.13108799072916E-13));
#24494=DIRECTION('',(0.189038743476622,0.981969629604083,-1.13108799072916E-13));
#24495=DIRECTION('',(1.00515054169548E-26,-1.1518563880486E-13,-1.));
#24496=DIRECTION('center_axis',(1.00515054169548E-26,-1.1518563880486E-13,
-1.));
#24497=DIRECTION('ref_axis',(8.72635297355373E-14,-1.,1.1518563880486E-13));
#24498=DIRECTION('',(0.177165010652742,-0.984181161677267,1.13363535807507E-13));
#24499=DIRECTION('',(0.181426836203858,0.983404445335213,-1.13274069239474E-13));
#24500=DIRECTION('',(-0.148350608954417,0.988934829411349,-1.13911090062123E-13));
#24501=DIRECTION('center_axis',(-0.983404445335213,0.181426836203859,-2.0897766024496E-14));
#24502=DIRECTION('ref_axis',(0.181426836203859,0.983404445335213,-1.13274069239474E-13));
#24503=DIRECTION('',(0.181426836203858,0.983404445335213,-1.13274069239474E-13));
#24504=DIRECTION('',(1.00515054169548E-26,-1.1518563880486E-13,-1.));
#24505=DIRECTION('center_axis',(1.00515054169548E-26,-1.1518563880486E-13,
-1.));
#24506=DIRECTION('ref_axis',(8.72635297355373E-14,-1.,1.1518563880486E-13));
#24507=DIRECTION('',(0.499999999998003,0.866025403785592,-9.97536893562752E-14));
#24508=DIRECTION('',(1.,8.72635297355373E-14,0.));
#24509=DIRECTION('',(0.499999999998154,-0.866025403785505,9.97536893562751E-14));
#24510=DIRECTION('',(1.,8.72635297355373E-14,0.));
#24511=DIRECTION('',(0.499999999998003,0.866025403785592,-9.97536893562752E-14));
#24512=DIRECTION('',(0.148350608954417,-0.988934829411349,1.13911090062123E-13));
#24513=DIRECTION('',(-0.18142683620403,0.983404445335182,-1.13274069239474E-13));
#24514=DIRECTION('',(0.148350608954245,0.988934829411375,-1.13911090062123E-13));
#24515=DIRECTION('',(0.499999999998154,-0.866025403785505,9.97536893562751E-14));
#24516=DIRECTION('',(1.,8.72635297355373E-14,0.));
#24517=DIRECTION('center_axis',(0.983404445335182,0.18142683620403,-2.0897766024496E-14));
#24518=DIRECTION('ref_axis',(0.18142683620403,-0.983404445335182,1.13274069239474E-13));
#24519=DIRECTION('',(-0.18142683620403,0.983404445335181,-1.13274069239474E-13));
#24520=DIRECTION('',(-1.00515054169548E-26,1.1518563880486E-13,1.));
#24521=DIRECTION('center_axis',(1.00515054169548E-26,-1.1518563880486E-13,
-1.));
#24522=DIRECTION('ref_axis',(8.72635297355373E-14,-1.,1.1518563880486E-13));
#24523=DIRECTION('',(0.17716501065257,0.984181161677298,-1.13363535807507E-13));
#24524=DIRECTION('',(-0.148350608954245,-0.988934829411375,1.13911090062123E-13));
#24525=DIRECTION('',(-0.189038743476793,0.98196962960405,-1.13108799072916E-13));
#24526=DIRECTION('center_axis',(0.98196962960405,0.189038743476793,-2.17745484262326E-14));
#24527=DIRECTION('ref_axis',(0.189038743476793,-0.98196962960405,1.13108799072916E-13));
#24528=DIRECTION('',(0.189038743476793,-0.98196962960405,1.13108799072916E-13));
#24529=DIRECTION('',(-1.00515054169548E-26,1.1518563880486E-13,1.));
#24530=DIRECTION('center_axis',(1.00515054169548E-26,-1.1518563880486E-13,
-1.));
#24531=DIRECTION('ref_axis',(8.72635297355373E-14,-1.,1.1518563880486E-13));
#24532=DIRECTION('',(0.148350608954245,0.988934829411375,-1.13911090062123E-13));
#24533=DIRECTION('',(-0.17716501065257,-0.984181161677298,1.13363535807507E-13));
#24534=DIRECTION('',(-0.18142683620403,0.983404445335182,-1.13274069239474E-13));
#24535=DIRECTION('center_axis',(0.983404445335182,0.18142683620403,-2.0897766024496E-14));
#24536=DIRECTION('ref_axis',(0.18142683620403,-0.983404445335182,1.13274069239474E-13));
#24537=DIRECTION('',(0.18142683620403,-0.983404445335181,1.13274069239474E-13));
#24538=DIRECTION('',(-1.00515054169548E-26,1.1518563880486E-13,1.));
#24539=DIRECTION('center_axis',(1.00515054169548E-26,-1.1518563880486E-13,
-1.));
#24540=DIRECTION('ref_axis',(8.72635297355373E-14,-1.,1.1518563880486E-13));
#24541=DIRECTION('',(-0.499999999998154,0.866025403785505,-9.97536893562751E-14));
#24542=DIRECTION('',(-0.148350608954245,-0.988934829411375,1.13911090062123E-13));
#24543=DIRECTION('',(-0.133254699246801,0.991081825647431,-1.14158393195087E-13));
#24544=DIRECTION('',(-8.72635297355373E-14,1.,-1.1518563880486E-13));
#24545=DIRECTION('',(-1.,-8.72635297355373E-14,0.));
#24546=DIRECTION('center_axis',(1.,8.72635297355373E-14,0.));
#24547=DIRECTION('ref_axis',(8.72635297355373E-14,-1.,1.1518563880486E-13));
#24548=DIRECTION('',(8.72635297355373E-14,-1.,1.1518563880486E-13));
#24549=DIRECTION('',(1.00515054169548E-26,-1.1518563880486E-13,-1.));
#24550=DIRECTION('',(-1.00515054169548E-26,1.1518563880486E-13,1.));
#24551=DIRECTION('center_axis',(1.00515054169548E-26,-1.1518563880486E-13,
-1.));
#24552=DIRECTION('ref_axis',(8.67361737988403E-14,-1.,1.1518563880486E-13));
#24553=DIRECTION('center_axis',(-1.00515054169548E-26,1.1518563880486E-13,
1.));
#24554=DIRECTION('ref_axis',(8.90491384334761E-14,-1.,1.1518563880486E-13));
#24555=DIRECTION('',(-1.00515054169548E-26,1.1518563880486E-13,1.));
#24556=DIRECTION('',(1.00515054169548E-26,-1.1518563880486E-13,-1.));
#24557=DIRECTION('center_axis',(1.00515054169548E-26,-1.1518563880486E-13,
-1.));
#24558=DIRECTION('ref_axis',(8.67361737988404E-14,-1.,1.1518563880486E-13));
#24559=DIRECTION('center_axis',(-1.00515054169548E-26,1.1518563880486E-13,
1.));
#24560=DIRECTION('ref_axis',(8.67361737988404E-14,-1.,1.1518563880486E-13));
#24561=DIRECTION('',(-1.00515054169548E-26,1.1518563880486E-13,1.));
#24562=DIRECTION('',(1.00515054169548E-26,-1.1518563880486E-13,-1.));
#24563=DIRECTION('center_axis',(1.00515054169548E-26,-1.1518563880486E-13,
-1.));
#24564=DIRECTION('ref_axis',(8.67361737988403E-14,-1.,1.1518563880486E-13));
#24565=DIRECTION('center_axis',(-1.00515054169548E-26,1.1518563880486E-13,
1.));
#24566=DIRECTION('ref_axis',(8.67361737988404E-14,-1.,1.1518563880486E-13));
#24567=DIRECTION('',(-1.00515054169548E-26,1.1518563880486E-13,1.));
#24568=DIRECTION('',(1.00515054169548E-26,-1.1518563880486E-13,-1.));
#24569=DIRECTION('center_axis',(-1.,-8.72635297355373E-14,0.));
#24570=DIRECTION('ref_axis',(-8.72635297355373E-14,1.,-1.1518563880486E-13));
#24571=DIRECTION('',(-8.72635297355373E-14,1.,-1.1518563880486E-13));
#24572=DIRECTION('',(-1.00515054169548E-26,1.1518563880486E-13,1.));
#24573=DIRECTION('',(-1.00515054169548E-26,1.1518563880486E-13,1.));
#24574=DIRECTION('',(1.00515054169548E-26,-1.1518563880486E-13,-1.));
#24575=DIRECTION('',(-8.72635297355373E-14,1.,-1.1518563880486E-13));
#24576=DIRECTION('',(-8.72635297355373E-14,1.,-1.1518563880486E-13));
#24577=DIRECTION('center_axis',(-0.991081825647454,0.133254699246628,-1.53490276564824E-14));
#24578=DIRECTION('ref_axis',(0.133254699246628,0.991081825647454,-1.14158393195087E-13));
#24579=DIRECTION('',(0.133254699246629,0.991081825647454,-1.14158393195087E-13));
#24580=DIRECTION('',(-1.00515054169548E-26,1.1518563880486E-13,1.));
#24581=DIRECTION('center_axis',(-8.72635297355373E-14,1.,-1.1518563880486E-13));
#24582=DIRECTION('ref_axis',(1.00515054169548E-26,-1.1518563880486E-13,
-1.));
#24583=DIRECTION('',(1.,8.72635297355373E-14,0.));
#24584=DIRECTION('center_axis',(-8.69573680357505E-14,1.,-1.11694157466017E-13));
#24585=DIRECTION('ref_axis',(9.74682643132155E-27,-1.11694157466017E-13,
-1.));
#24586=DIRECTION('',(1.,8.72635297355373E-14,0.));
#24587=DIRECTION('center_axis',(-8.72635297355373E-14,1.,-1.1518563880486E-13));
#24588=DIRECTION('ref_axis',(1.00515054169548E-26,-1.1518563880486E-13,
-1.));
#24589=DIRECTION('',(1.,8.72635297355373E-14,0.));
#24590=DIRECTION('',(-1.00515054169548E-26,1.1518563880486E-13,1.));
#24591=DIRECTION('center_axis',(0.991081825647431,0.133254699246801,-1.53490276564823E-14));
#24592=DIRECTION('ref_axis',(0.133254699246801,-0.991081825647431,1.14158393195087E-13));
#24593=DIRECTION('',(0.133254699246801,-0.991081825647431,1.14158393195087E-13));
#24594=DIRECTION('',(-1.00515054169548E-26,1.1518563880486E-13,1.));
#24595=DIRECTION('center_axis',(1.,8.72635297355373E-14,0.));
#24596=DIRECTION('ref_axis',(8.72635297355373E-14,-1.,1.1518563880486E-13));
#24597=DIRECTION('',(-1.00515054169548E-26,1.1518563880486E-13,1.));
#24598=DIRECTION('',(8.72635297355373E-14,-1.,1.1518563880486E-13));
#24599=DIRECTION('',(-1.00515054169548E-26,1.1518563880486E-13,1.));
#24600=DIRECTION('',(8.72635297355373E-14,-1.,1.1518563880486E-13));
#24601=DIRECTION('',(1.00515054169548E-26,-1.1518563880486E-13,-1.));
#24602=DIRECTION('center_axis',(1.00515054169548E-26,-1.1518563880486E-13,
-1.));
#24603=DIRECTION('ref_axis',(8.67361737988404E-14,-1.,1.1518563880486E-13));
#24604=DIRECTION('center_axis',(-1.00515054169548E-26,1.1518563880486E-13,
1.));
#24605=DIRECTION('ref_axis',(8.78926561161582E-14,-1.,1.1518563880486E-13));
#24606=DIRECTION('center_axis',(1.00515054169548E-26,-1.1518563880486E-13,
-1.));
#24607=DIRECTION('ref_axis',(8.72370886447792E-14,-1.,1.1518563880486E-13));
#24608=DIRECTION('center_axis',(-1.00515054169548E-26,1.1518563880486E-13,
1.));
#24609=DIRECTION('ref_axis',(8.72370886447792E-14,-1.,1.1518563880486E-13));
#24610=DIRECTION('center_axis',(1.00515054169548E-26,-1.1518563880486E-13,
-1.));
#24611=DIRECTION('ref_axis',(-8.80292434753227E-14,1.,-1.1518563880486E-13));
#24612=DIRECTION('center_axis',(-1.00515054169548E-26,1.1518563880486E-13,
1.));
#24613=DIRECTION('ref_axis',(8.54871728961371E-14,-1.,1.1518563880486E-13));
#24614=DIRECTION('center_axis',(1.00515054169548E-26,-1.1518563880486E-13,
-1.));
#24615=DIRECTION('ref_axis',(8.72370886447792E-14,-1.,1.1518563880486E-13));
#24616=DIRECTION('center_axis',(-1.00515054169548E-26,1.1518563880486E-13,
1.));
#24617=DIRECTION('ref_axis',(8.90504802424435E-14,-1.,1.1518563880486E-13));
#24618=DIRECTION('center_axis',(1.00515054169548E-26,-1.1518563880486E-13,
-1.));
#24619=DIRECTION('ref_axis',(8.72635297355373E-14,-1.,1.1518563880486E-13));
#24620=DIRECTION('center_axis',(-1.00515054169548E-26,1.1518563880486E-13,
1.));
#24621=DIRECTION('ref_axis',(5.08482145278322E-14,-1.,1.1518563880486E-13));
#24622=DIRECTION('center_axis',(-8.72635297355373E-14,1.,-1.1518563880486E-13));
#24623=DIRECTION('ref_axis',(1.00515054169548E-26,-1.1518563880486E-13,
-1.));
#24624=DIRECTION('',(1.,8.72635297355373E-14,0.));
#24625=DIRECTION('',(-1.00515054169548E-26,1.1518563880486E-13,1.));
#24626=DIRECTION('',(-1.,-8.72635297355373E-14,0.));
#24627=DIRECTION('',(1.00515054169548E-26,-1.1518563880486E-13,-1.));
#24628=DIRECTION('center_axis',(0.866025403785505,0.499999999998154,-5.75928194022086E-14));
#24629=DIRECTION('ref_axis',(0.499999999998154,-0.866025403785505,9.97536893562752E-14));
#24630=DIRECTION('',(0.499999999998154,-0.866025403785505,9.97536893562751E-14));
#24631=DIRECTION('',(-1.00515054169548E-26,1.1518563880486E-13,1.));
#24632=DIRECTION('',(-0.499999999998154,0.866025403785505,-9.97536893562751E-14));
#24633=DIRECTION('center_axis',(-0.866025403785592,0.499999999998003,-5.75928194022086E-14));
#24634=DIRECTION('ref_axis',(0.499999999998003,0.866025403785592,-9.97536893562752E-14));
#24635=DIRECTION('',(0.499999999998002,0.866025403785592,-9.97536893562751E-14));
#24636=DIRECTION('',(1.00515054169548E-26,-1.1518563880486E-13,-1.));
#24637=DIRECTION('center_axis',(-0.988934829411349,-0.148350608954417,1.70878596594946E-14));
#24638=DIRECTION('ref_axis',(-0.148350608954417,0.988934829411349,-1.13911090062123E-13));
#24639=DIRECTION('',(1.00515054169548E-26,-1.1518563880486E-13,-1.));
#24640=DIRECTION('center_axis',(-0.984181161677267,-0.177165010652742,2.0406864925896E-14));
#24641=DIRECTION('ref_axis',(-0.177165010652742,0.984181161677267,-1.13363535807507E-13));
#24642=DIRECTION('',(1.00515054169548E-26,-1.1518563880486E-13,-1.));
#24643=DIRECTION('center_axis',(-0.988934829411349,-0.148350608954417,1.70878596594946E-14));
#24644=DIRECTION('ref_axis',(-0.148350608954417,0.988934829411349,-1.13911090062123E-13));
#24645=DIRECTION('',(1.00515054169548E-26,-1.1518563880486E-13,-1.));
#24646=DIRECTION('',(1.00515054169548E-26,-1.1518563880486E-13,-1.));
#24647=DIRECTION('center_axis',(-0.866025403785592,0.499999999998003,-5.75928194022086E-14));
#24648=DIRECTION('ref_axis',(0.499999999998003,0.866025403785592,-9.97536893562752E-14));
#24649=DIRECTION('',(0.499999999998002,0.866025403785592,-9.97536893562751E-14));
#24650=DIRECTION('',(1.00515054169548E-26,-1.1518563880486E-13,-1.));
#24651=DIRECTION('',(-1.00515054169548E-26,1.1518563880486E-13,1.));
#24652=DIRECTION('center_axis',(-8.72635297355373E-14,1.,-1.1518563880486E-13));
#24653=DIRECTION('ref_axis',(1.00515054169548E-26,-1.1518563880486E-13,
-1.));
#24654=DIRECTION('',(1.,8.72635297355373E-14,0.));
#24655=DIRECTION('',(-1.00515054169548E-26,1.1518563880486E-13,1.));
#24656=DIRECTION('center_axis',(0.866025403785505,0.499999999998154,-5.75928194022086E-14));
#24657=DIRECTION('ref_axis',(0.499999999998154,-0.866025403785505,9.97536893562752E-14));
#24658=DIRECTION('',(0.499999999998154,-0.866025403785505,9.97536893562751E-14));
#24659=DIRECTION('',(-1.00515054169548E-26,1.1518563880486E-13,1.));
#24660=DIRECTION('center_axis',(8.72635297355373E-14,-1.,1.1518563880486E-13));
#24661=DIRECTION('ref_axis',(-1.00515054169548E-26,1.1518563880486E-13,
1.));
#24662=DIRECTION('',(1.00515054169548E-26,-1.1518563880486E-13,-1.));
#24663=DIRECTION('',(1.,8.72635297355373E-14,0.));
#24664=DIRECTION('',(-1.00515054169548E-26,1.1518563880486E-13,1.));
#24665=DIRECTION('center_axis',(-0.866025403785592,0.499999999998003,-5.75928194022086E-14));
#24666=DIRECTION('ref_axis',(0.499999999998003,0.866025403785592,-9.97536893562752E-14));
#24667=DIRECTION('',(0.499999999998002,0.866025403785592,-9.97536893562752E-14));
#24668=DIRECTION('',(1.00515054169548E-26,-1.1518563880486E-13,-1.));
#24669=DIRECTION('',(-1.00515054169548E-26,1.1518563880486E-13,1.));
#24670=DIRECTION('center_axis',(-8.72635297355373E-14,1.,-1.1518563880486E-13));
#24671=DIRECTION('ref_axis',(1.00515054169548E-26,-1.1518563880486E-13,
-1.));
#24672=DIRECTION('',(1.,8.72635297355373E-14,0.));
#24673=DIRECTION('',(-1.00515054169548E-26,1.1518563880486E-13,1.));
#24674=DIRECTION('center_axis',(0.866025403785505,0.499999999998154,-5.75928194022086E-14));
#24675=DIRECTION('ref_axis',(0.499999999998154,-0.866025403785505,9.97536893562752E-14));
#24676=DIRECTION('',(0.499999999998153,-0.866025403785505,9.97536893562752E-14));
#24677=DIRECTION('',(-1.00515054169548E-26,1.1518563880486E-13,1.));
#24678=DIRECTION('center_axis',(0.988934829411375,-0.148350608954245,1.70878596594946E-14));
#24679=DIRECTION('ref_axis',(-0.148350608954245,-0.988934829411375,1.13911090062123E-13));
#24680=DIRECTION('',(-1.00515054169548E-26,1.1518563880486E-13,1.));
#24681=DIRECTION('center_axis',(0.984181161677298,-0.17716501065257,2.0406864925896E-14));
#24682=DIRECTION('ref_axis',(-0.17716501065257,-0.984181161677298,1.13363535807507E-13));
#24683=DIRECTION('',(-1.00515054169548E-26,1.1518563880486E-13,1.));
#24684=DIRECTION('center_axis',(0.988934829411375,-0.148350608954245,1.70878596594946E-14));
#24685=DIRECTION('ref_axis',(-0.148350608954245,-0.988934829411375,1.13911090062123E-13));
#24686=DIRECTION('',(-1.00515054169548E-26,1.1518563880486E-13,1.));
#24687=DIRECTION('center_axis',(-8.72635297355373E-14,1.,-1.1518563880486E-13));
#24688=DIRECTION('ref_axis',(1.00515054169548E-26,-1.1518563880486E-13,
-1.));
#24689=DIRECTION('',(1.,8.72635297355373E-14,0.));
#24690=DIRECTION('',(-1.00515054169548E-26,1.1518563880486E-13,1.));
#24691=DIRECTION('',(-1.,-8.72635297355373E-14,0.));
#24692=DIRECTION('',(1.00515054169548E-26,-1.1518563880486E-13,-1.));
#24693=DIRECTION('center_axis',(0.866025403785505,0.499999999998154,-5.75928194022086E-14));
#24694=DIRECTION('ref_axis',(0.499999999998154,-0.866025403785505,9.97536893562752E-14));
#24695=DIRECTION('',(0.499999999998153,-0.866025403785505,9.97536893562752E-14));
#24696=DIRECTION('',(-1.00515054169548E-26,1.1518563880486E-13,1.));
#24697=DIRECTION('center_axis',(-0.866025403785592,0.499999999998003,-5.75928194022086E-14));
#24698=DIRECTION('ref_axis',(0.499999999998003,0.866025403785592,-9.97536893562752E-14));
#24699=DIRECTION('',(0.499999999998002,0.866025403785592,-9.97536893562752E-14));
#24700=DIRECTION('',(-0.499999999998002,-0.866025403785592,9.97536893562752E-14));
#24701=DIRECTION('',(1.00515054169548E-26,-1.1518563880486E-13,-1.));
#24702=DIRECTION('center_axis',(1.00515054169548E-26,-1.1518563880486E-13,
-1.));
#24703=DIRECTION('ref_axis',(8.72635297355373E-14,-1.,1.1518563880486E-13));
#24704=DIRECTION('',(-8.72635297355373E-14,1.,-1.1518563880486E-13));
#24705=DIRECTION('',(-1.,-8.72635297355373E-14,0.));
#24706=DIRECTION('',(8.72635297355373E-14,-1.,1.1518563880486E-13));
#24707=DIRECTION('center_axis',(1.,8.72635297355373E-14,0.));
#24708=DIRECTION('ref_axis',(8.72635297355373E-14,-1.,1.1518563880486E-13));
#24709=DIRECTION('',(8.72635297355373E-14,-1.,1.1518563880486E-13));
#24710=DIRECTION('',(-1.00515054169548E-26,1.1518563880486E-13,1.));
#24711=DIRECTION('center_axis',(1.00515054169548E-26,-1.1518563880486E-13,
-1.));
#24712=DIRECTION('ref_axis',(8.72635297355373E-14,-1.,1.1518563880486E-13));
#24713=DIRECTION('',(-8.72635297355373E-14,1.,-1.1518563880486E-13));
#24714=DIRECTION('',(-1.,-8.72635297355373E-14,0.));
#24715=DIRECTION('center_axis',(-1.,-8.72635297355373E-14,0.));
#24716=DIRECTION('ref_axis',(-8.72635297355373E-14,1.,-1.1518563880486E-13));
#24717=DIRECTION('',(-8.72635297355373E-14,1.,-1.1518563880486E-13));
#24718=DIRECTION('',(1.00515054169548E-26,-1.1518563880486E-13,-1.));
#24719=DIRECTION('center_axis',(1.00515054169548E-26,-1.1518563880486E-13,
-1.));
#24720=DIRECTION('ref_axis',(8.72635297355373E-14,-1.,1.1518563880486E-13));
#24721=DIRECTION('',(-8.72635297355373E-14,1.,-1.1518563880486E-13));
#24722=DIRECTION('',(1.,8.72635297355373E-14,0.));
#24723=DIRECTION('center_axis',(1.,8.72635297355373E-14,0.));
#24724=DIRECTION('ref_axis',(8.72635297355373E-14,-1.,1.1518563880486E-13));
#24725=DIRECTION('',(-8.72635297355373E-14,1.,-1.1518563880486E-13));
#24726=DIRECTION('',(-1.00515054169548E-26,1.1518563880486E-13,1.));
#24727=DIRECTION('center_axis',(1.00515054169548E-26,-1.1518563880486E-13,
-1.));
#24728=DIRECTION('ref_axis',(8.72635297355373E-14,-1.,1.1518563880486E-13));
#24729=DIRECTION('',(-8.72635297355373E-14,1.,-1.1518563880486E-13));
#24730=DIRECTION('',(1.,8.72635297355373E-14,0.));
#24731=DIRECTION('center_axis',(-1.,-8.72635297355373E-14,0.));
#24732=DIRECTION('ref_axis',(-8.72635297355373E-14,1.,-1.1518563880486E-13));
#24733=DIRECTION('',(-8.72635297355373E-14,1.,-1.1518563880486E-13));
#24734=DIRECTION('',(1.00515054169548E-26,-1.1518563880486E-13,-1.));
#24735=DIRECTION('center_axis',(1.00515054169548E-26,-1.1518563880486E-13,
-1.));
#24736=DIRECTION('ref_axis',(8.72635297355373E-14,-1.,1.1518563880486E-13));
#24737=DIRECTION('',(-8.72635297355373E-14,1.,-1.1518563880486E-13));
#24738=DIRECTION('',(1.,8.72635297355373E-14,0.));
#24739=DIRECTION('center_axis',(1.,8.72635297355373E-14,0.));
#24740=DIRECTION('ref_axis',(8.72635297355373E-14,-1.,1.1518563880486E-13));
#24741=DIRECTION('',(8.72635297355373E-14,-1.,1.1518563880486E-13));
#24742=DIRECTION('',(-1.00515054169548E-26,1.1518563880486E-13,1.));
#24743=DIRECTION('center_axis',(1.00515054169548E-26,-1.1518563880486E-13,
-1.));
#24744=DIRECTION('ref_axis',(8.72635297355373E-14,-1.,1.1518563880486E-13));
#24745=DIRECTION('',(-8.72635297355373E-14,1.,-1.1518563880486E-13));
#24746=DIRECTION('',(-1.,-8.72635297355373E-14,0.));
#24747=DIRECTION('center_axis',(-1.,-8.72635297355373E-14,0.));
#24748=DIRECTION('ref_axis',(-8.72635297355373E-14,1.,-1.1518563880486E-13));
#24749=DIRECTION('',(1.00515054169548E-26,-1.1518563880486E-13,-1.));
#24750=DIRECTION('center_axis',(8.72635297355373E-14,-1.,1.1518563880486E-13));
#24751=DIRECTION('ref_axis',(-1.00515054169548E-26,1.1518563880486E-13,
1.));
#24752=DIRECTION('axis',(0.,0.,1.));
#24753=DIRECTION('refdir',(1.,0.,0.));
#24754=DIRECTION('center_axis',(1.,0.,0.));
#24755=DIRECTION('ref_axis',(0.,0.,-1.));
#24756=DIRECTION('center_axis',(1.,0.,0.));
#24757=DIRECTION('ref_axis',(0.,0.,-1.));
#24758=DIRECTION('center_axis',(1.,0.,0.));
#24759=DIRECTION('ref_axis',(0.,0.,-1.));
#24760=DIRECTION('center_axis',(0.,1.,1.22464679914735E-16));
#24761=DIRECTION('ref_axis',(0.,-1.22464679914735E-16,1.));
#24762=DIRECTION('center_axis',(-1.,0.,0.));
#24763=DIRECTION('ref_axis',(0.,0.,-1.));
#24764=DIRECTION('center_axis',(-1.,0.,0.));
#24765=DIRECTION('ref_axis',(0.,0.,1.));
#24766=DIRECTION('center_axis',(-1.,0.,0.));
#24767=DIRECTION('ref_axis',(0.,0.,1.));
#24768=DIRECTION('center_axis',(-1.,0.,0.));
#24769=DIRECTION('ref_axis',(0.,0.,1.));
#24770=DIRECTION('center_axis',(-1.,0.,0.));
#24771=DIRECTION('ref_axis',(0.,0.,1.));
#24772=DIRECTION('',(1.,0.,0.));
#24773=DIRECTION('center_axis',(1.,0.,0.));
#24774=DIRECTION('ref_axis',(0.,0.,-1.));
#24775=DIRECTION('center_axis',(-1.,0.,0.));
#24776=DIRECTION('ref_axis',(0.,0.,1.));
#24777=DIRECTION('center_axis',(-1.,0.,0.));
#24778=DIRECTION('ref_axis',(0.,0.,1.));
#24779=DIRECTION('center_axis',(-1.,0.,0.));
#24780=DIRECTION('ref_axis',(0.,0.,1.));
#24781=DIRECTION('center_axis',(-1.,0.,0.));
#24782=DIRECTION('ref_axis',(0.,0.,1.));
#24783=DIRECTION('center_axis',(-1.,0.,0.));
#24784=DIRECTION('ref_axis',(0.,0.,1.));
#24785=DIRECTION('',(0.707106781186551,8.65956056235488E-17,0.707106781186544));
#24786=DIRECTION('center_axis',(-1.,0.,0.));
#24787=DIRECTION('ref_axis',(0.,0.,1.));
#24788=DIRECTION('center_axis',(-1.,0.,0.));
#24789=DIRECTION('ref_axis',(0.,0.,1.));
#24790=DIRECTION('',(1.,0.,0.));
#24791=DIRECTION('center_axis',(1.,0.,0.));
#24792=DIRECTION('ref_axis',(0.,0.,-1.));
#24793=DIRECTION('center_axis',(-1.,0.,0.));
#24794=DIRECTION('ref_axis',(0.,0.,1.));
#24795=DIRECTION('center_axis',(1.,0.,0.));
#24796=DIRECTION('ref_axis',(0.,0.,-1.));
#24797=DIRECTION('',(0.,0.500000000000001,0.866025403784438));
#24798=DIRECTION('',(0.,1.,1.07308185624083E-16));
#24799=DIRECTION('center_axis',(1.,0.,0.));
#24800=DIRECTION('ref_axis',(0.,0.,-1.));
#24801=DIRECTION('',(0.,0.500000000000001,0.866025403784438));
#24802=DIRECTION('',(0.,-0.500000000000001,0.866025403784438));
#24803=DIRECTION('center_axis',(1.,0.,0.));
#24804=DIRECTION('ref_axis',(0.,0.,-1.));
#24805=DIRECTION('',(0.,-0.500000000000001,0.866025403784438));
#24806=DIRECTION('',(0.,-1.,0.));
#24807=DIRECTION('center_axis',(1.,0.,0.));
#24808=DIRECTION('ref_axis',(0.,0.,-1.));
#24809=DIRECTION('',(0.,-1.,0.));
#24810=DIRECTION('',(0.,-0.500000000000002,-0.866025403784437));
#24811=DIRECTION('center_axis',(1.,0.,0.));
#24812=DIRECTION('ref_axis',(0.,0.,-1.));
#24813=DIRECTION('',(0.,-0.500000000000002,-0.866025403784437));
#24814=DIRECTION('',(0.,0.5,-0.866025403784438));
#24815=DIRECTION('center_axis',(1.,0.,0.));
#24816=DIRECTION('ref_axis',(0.,0.,-1.));
#24817=DIRECTION('',(0.,0.5,-0.866025403784438));
#24818=DIRECTION('',(0.,1.,1.07308185624083E-16));
#24819=DIRECTION('center_axis',(1.,0.,0.));
#24820=DIRECTION('ref_axis',(0.,0.,-1.));
#24821=DIRECTION('center_axis',(1.,0.,0.));
#24822=DIRECTION('ref_axis',(0.,0.,-1.));
#24823=DIRECTION('center_axis',(1.,0.,0.));
#24824=DIRECTION('ref_axis',(0.,0.,-1.));
#24825=DIRECTION('center_axis',(1.,0.,0.));
#24826=DIRECTION('ref_axis',(0.,0.,-1.));
#24827=DIRECTION('center_axis',(1.,0.,0.));
#24828=DIRECTION('ref_axis',(0.,0.,-1.));
#24829=DIRECTION('center_axis',(-1.,0.,0.));
#24830=DIRECTION('ref_axis',(0.,0.,1.));
#24831=DIRECTION('center_axis',(1.,0.,0.));
#24832=DIRECTION('ref_axis',(0.,0.,-1.));
#24833=DIRECTION('center_axis',(1.,0.,0.));
#24834=DIRECTION('ref_axis',(0.,0.,-1.));
#24835=DIRECTION('center_axis',(1.,0.,0.));
#24836=DIRECTION('ref_axis',(0.,0.,-1.));
#24837=DIRECTION('center_axis',(1.,0.,0.));
#24838=DIRECTION('ref_axis',(0.,0.,-1.));
#24839=DIRECTION('center_axis',(1.,0.,0.));
#24840=DIRECTION('ref_axis',(0.,0.,-1.));
#24841=DIRECTION('center_axis',(1.,0.,0.));
#24842=DIRECTION('ref_axis',(0.,0.,-1.));
#24843=DIRECTION('center_axis',(1.,0.,0.));
#24844=DIRECTION('ref_axis',(0.,0.,-1.));
#24845=DIRECTION('center_axis',(0.,-1.07308185624083E-16,1.));
#24846=DIRECTION('ref_axis',(0.,-1.,-1.07308185624083E-16));
#24847=DIRECTION('',(-1.,0.,0.));
#24848=DIRECTION('',(-1.,0.,0.));
#24849=DIRECTION('center_axis',(0.,0.866025403784438,0.5));
#24850=DIRECTION('ref_axis',(0.,-0.5,0.866025403784438));
#24851=DIRECTION('',(-1.,0.,0.));
#24852=DIRECTION('center_axis',(0.,0.866025403784438,-0.500000000000002));
#24853=DIRECTION('ref_axis',(0.,0.500000000000002,0.866025403784438));
#24854=DIRECTION('',(-1.,0.,0.));
#24855=DIRECTION('center_axis',(0.,0.,-1.));
#24856=DIRECTION('ref_axis',(-1.,0.,0.));
#24857=DIRECTION('',(-1.,0.,0.));
#24858=DIRECTION('center_axis',(0.,-0.866025403784438,-0.500000000000001));
#24859=DIRECTION('ref_axis',(0.,0.500000000000001,-0.866025403784438));
#24860=DIRECTION('',(-1.,0.,0.));
#24861=DIRECTION('center_axis',(0.,-0.866025403784438,0.500000000000001));
#24862=DIRECTION('ref_axis',(0.,-0.500000000000001,-0.866025403784438));
#24863=DIRECTION('',(0.,0.,1.));
#24864=DIRECTION('',(1.,0.,0.));
#24865=DIRECTION('',(0.,0.,1.));
#24866=DIRECTION('',(1.,0.,0.));
#24867=DIRECTION('',(0.,0.,1.));
#24868=DIRECTION('',(1.,0.,0.));
#24869=DIRECTION('',(0.,0.,1.));
#24870=DIRECTION('',(1.,0.,0.));
#24871=DIRECTION('',(0.,0.,1.));
#24872=DIRECTION('',(1.,0.,0.));
#24873=DIRECTION('',(0.,0.,1.));
#24874=DIRECTION('',(1.,0.,0.));
#24875=DIRECTION('',(1.,0.,0.));
#24876=DIRECTION('',(0.,0.,-1.));
#24877=DIRECTION('',(0.913545457642601,0.406736643075801,0.));
#24878=DIRECTION('',(0.,0.,-1.));
#24879=DIRECTION('',(0.669130606358857,0.743144825477395,0.));
#24880=DIRECTION('',(0.,0.,-1.));
#24881=DIRECTION('',(0.309016994374945,0.951056516295154,0.));
#24882=DIRECTION('',(0.,0.,-1.));
#24883=DIRECTION('',(-0.104528463267657,0.994521895368273,0.));
#24884=DIRECTION('',(0.,0.,-1.));
#24885=DIRECTION('',(-0.500000000000004,0.866025403784436,0.));
#24886=DIRECTION('',(0.,0.,-1.));
#24887=DIRECTION('',(-0.809016994374951,0.587785252292469,0.));
#24888=DIRECTION('',(0.,0.,-1.));
#24889=DIRECTION('',(-0.978147600733807,0.207911690817753,0.));
#24890=DIRECTION('',(0.,0.,-1.));
#24891=DIRECTION('',(-0.978147600733804,-0.207911690817766,0.));
#24892=DIRECTION('',(0.,0.,-1.));
#24893=DIRECTION('',(-0.809016994374943,-0.58778525229248,0.));
#24894=DIRECTION('',(0.,0.,-1.));
#24895=DIRECTION('',(-0.499999999999992,-0.866025403784443,0.));
#24896=DIRECTION('',(0.,0.,-1.));
#24897=DIRECTION('',(-0.104528463267644,-0.994521895368274,0.));
#24898=DIRECTION('',(0.,0.,-1.));
#24899=DIRECTION('',(0.309016994374957,-0.95105651629515,0.));
#24900=DIRECTION('',(0.,0.,-1.));
#24901=DIRECTION('',(0.669130606358867,-0.743144825477386,0.));
#24902=DIRECTION('',(0.,0.,-1.));
#24903=DIRECTION('',(0.913545457642606,-0.406736643075789,0.));
#24904=DIRECTION('',(0.,0.,-1.));
#24905=CARTESIAN_POINT('',(0.,0.,0.));
#24906=CARTESIAN_POINT('',(0.,0.,0.));
#24907=CARTESIAN_POINT('Origin',(0.,0.,-50.));
#24908=CARTESIAN_POINT('',(-30.,-3.67394039744206E-15,-55.));
#24909=CARTESIAN_POINT('Origin',(0.,0.,-55.));
#24910=CARTESIAN_POINT('',(-25.,-3.06161699786838E-15,-50.));
#24911=CARTESIAN_POINT('Origin',(-30.,-3.67394039744206E-15,-50.));
#24912=CARTESIAN_POINT('Origin',(0.,0.,-50.));
#24913=CARTESIAN_POINT('Origin',(0.,0.,-50.));
#24914=CARTESIAN_POINT('',(250.,3.06161699786838E-14,-50.));
#24915=CARTESIAN_POINT('',(-250.,-3.06161699786838E-14,-50.));
#24916=CARTESIAN_POINT('Origin',(0.,0.,-50.));
#24917=CARTESIAN_POINT('Origin',(0.,0.,-50.));
#24918=CARTESIAN_POINT('',(-245.,-3.00038465791102E-14,-55.));
#24919=CARTESIAN_POINT('Origin',(-245.,-3.00038465791102E-14,-50.));
#24920=CARTESIAN_POINT('Origin',(0.,0.,-55.));
#24921=CARTESIAN_POINT('Origin',(0.,0.,-35.));
#24922=CARTESIAN_POINT('',(-34.8143500942353,3.60014270772951,-45.));
#24923=CARTESIAN_POINT('',(-31.4834665561195,-15.2902365452502,-45.));
#24924=CARTESIAN_POINT('Origin',(0.,0.,-45.));
#24925=CARTESIAN_POINT('',(-31.4834665561195,-15.2902365452502,-36.5156684558794));
#24926=CARTESIAN_POINT('',(-31.4834665561195,-15.2902365452502,-35.));
#24927=CARTESIAN_POINT('',(-28.9834665561195,-19.6203635641724,-36.5156684558794));
#24928=CARTESIAN_POINT('Origin',(0.,0.,-25.7404283258302));
#24929=CARTESIAN_POINT('',(-28.9834665561195,-19.6203635641724,-45.));
#24930=CARTESIAN_POINT('',(-28.9834665561195,-19.6203635641724,-35.));
#24931=CARTESIAN_POINT('',(-14.2893600049743,-31.9501829517178,-45.));
#24932=CARTESIAN_POINT('Origin',(0.,0.,-45.));
#24933=CARTESIAN_POINT('',(-14.2893600049743,-31.9501829517178,-36.5156684558794));
#24934=CARTESIAN_POINT('',(-14.2893600049743,-31.9501829517178,-35.));
#24935=CARTESIAN_POINT('',(-9.59089690104477,-33.6602836683462,-36.5156684558794));
#24936=CARTESIAN_POINT('Origin',(0.,0.,-25.7404283258302));
#24937=CARTESIAN_POINT('',(-9.59089690104477,-33.6602836683461,-45.));
#24938=CARTESIAN_POINT('',(-9.59089690104477,-33.6602836683462,-35.));
#24939=CARTESIAN_POINT('',(9.59089690104522,-33.660283668346,-45.));
#24940=CARTESIAN_POINT('Origin',(0.,0.,-45.));
#24941=CARTESIAN_POINT('',(9.59089690104522,-33.660283668346,-36.5156684558794));
#24942=CARTESIAN_POINT('',(9.59089690104522,-33.660283668346,-35.));
#24943=CARTESIAN_POINT('',(14.2893600049748,-31.9501829517176,-36.5156684558794));
#24944=CARTESIAN_POINT('Origin',(0.,0.,-25.7404283258302));
#24945=CARTESIAN_POINT('',(14.2893600049748,-31.9501829517176,-45.));
#24946=CARTESIAN_POINT('',(14.2893600049748,-31.9501829517176,-35.));
#24947=CARTESIAN_POINT('',(28.9834665561198,-19.620363564172,-45.));
#24948=CARTESIAN_POINT('Origin',(0.,0.,-45.));
#24949=CARTESIAN_POINT('',(28.9834665561198,-19.620363564172,-36.5156684558794));
#24950=CARTESIAN_POINT('',(28.9834665561198,-19.620363564172,-35.));
#24951=CARTESIAN_POINT('',(31.4834665561197,-15.2902365452498,-36.5156684558794));
#24952=CARTESIAN_POINT('Origin',(0.,0.,-25.7404283258302));
#24953=CARTESIAN_POINT('',(31.4834665561197,-15.2902365452498,-45.));
#24954=CARTESIAN_POINT('',(31.4834665561197,-15.2902365452498,-35.));
#24955=CARTESIAN_POINT('',(35.,-4.28626379701574E-15,-45.));
#24956=CARTESIAN_POINT('Origin',(0.,0.,-45.));
#24957=CARTESIAN_POINT('',(35.,-4.28626379701574E-15,-35.));
#24958=CARTESIAN_POINT('',(35.,-4.28626379701574E-15,-35.));
#24959=CARTESIAN_POINT('Origin',(0.,0.,-35.));
#24960=CARTESIAN_POINT('',(34.8143500942353,3.60014270772997,-45.));
#24961=CARTESIAN_POINT('Origin',(0.,0.,-45.));
#24962=CARTESIAN_POINT('',(34.8143500942353,3.60014270772997,-36.5156684558794));
#24963=CARTESIAN_POINT('',(34.8143500942353,3.60014270772997,-35.));
#24964=CARTESIAN_POINT('',(33.9461092059006,8.524181472791,-36.5156684558794));
#24965=CARTESIAN_POINT('Origin',(0.,0.,-25.7404283258302));
#24966=CARTESIAN_POINT('',(33.9461092059006,8.524181472791,-45.));
#24967=CARTESIAN_POINT('',(33.9461092059006,8.524181472791,-35.));
#24968=CARTESIAN_POINT('',(24.3552123048554,25.1361021955557,-45.));
#24969=CARTESIAN_POINT('Origin',(0.,0.,-45.));
#24970=CARTESIAN_POINT('',(24.3552123048554,25.1361021955557,-36.5156684558794));
#24971=CARTESIAN_POINT('',(24.3552123048554,25.1361021955557,-35.));
#24972=CARTESIAN_POINT('',(20.5249900892604,28.3500402439884,-36.5156684558794));
#24973=CARTESIAN_POINT('Origin',(0.,0.,-25.7404283258302));
#24974=CARTESIAN_POINT('',(20.5249900892604,28.3500402439884,-45.));
#24975=CARTESIAN_POINT('',(20.5249900892604,28.3500402439884,-35.));
#24976=CARTESIAN_POINT('',(2.5,34.9106001094224,-45.));
#24977=CARTESIAN_POINT('Origin',(0.,0.,-45.));
#24978=CARTESIAN_POINT('',(2.5,34.9106001094224,-36.5156684558794));
#24979=CARTESIAN_POINT('',(2.5,34.9106001094224,-35.));
#24980=CARTESIAN_POINT('',(-2.5,34.9106001094224,-36.5156684558794));
#24981=CARTESIAN_POINT('Origin',(0.,0.,-25.7404283258302));
#24982=CARTESIAN_POINT('',(-2.5,34.9106001094224,-45.));
#24983=CARTESIAN_POINT('',(-2.5,34.9106001094224,-35.));
#24984=CARTESIAN_POINT('',(-20.5249900892608,28.3500402439881,-45.));
#24985=CARTESIAN_POINT('Origin',(0.,0.,-45.));
#24986=CARTESIAN_POINT('',(-20.5249900892608,28.3500402439881,-36.5156684558794));
#24987=CARTESIAN_POINT('',(-20.5249900892608,28.3500402439881,-35.));
#24988=CARTESIAN_POINT('',(-24.3552123048557,25.1361021955554,-36.5156684558794));
#24989=CARTESIAN_POINT('Origin',(0.,0.,-25.7404283258302));
#24990=CARTESIAN_POINT('',(-24.3552123048557,25.1361021955554,-45.));
#24991=CARTESIAN_POINT('',(-24.3552123048557,25.1361021955554,-35.));
#24992=CARTESIAN_POINT('',(-33.9461092059007,8.52418147279055,-45.));
#24993=CARTESIAN_POINT('Origin',(0.,0.,-45.));
#24994=CARTESIAN_POINT('',(-33.9461092059007,8.52418147279055,-36.5156684558794));
#24995=CARTESIAN_POINT('',(-33.9461092059007,8.52418147279055,-35.));
#24996=CARTESIAN_POINT('',(-34.8143500942353,3.60014270772951,-36.5156684558794));
#24997=CARTESIAN_POINT('Origin',(0.,0.,-25.7404283258302));
#24998=CARTESIAN_POINT('',(-34.8143500942353,3.60014270772951,-35.));
#24999=CARTESIAN_POINT('Origin',(263.115760998171,-242.,-20.));
#25000=CARTESIAN_POINT('',(263.115760998171,-239.5,-20.));
#25001=CARTESIAN_POINT('Origin',(263.115760998171,-242.,-20.));
#25002=CARTESIAN_POINT('',(258.115760998171,-239.5,-20.));
#25003=CARTESIAN_POINT('',(263.115760998171,-239.5,-20.));
#25004=CARTESIAN_POINT('Origin',(258.115760998171,-242.,-20.));
#25005=CARTESIAN_POINT('Origin',(263.115760998171,-242.,20.));
#25006=CARTESIAN_POINT('',(263.115760998171,-239.5,20.));
#25007=CARTESIAN_POINT('Origin',(263.115760998171,-242.,20.));
#25008=CARTESIAN_POINT('',(258.115760998171,-239.5,20.));
#25009=CARTESIAN_POINT('',(263.115760998171,-239.5,20.));
#25010=CARTESIAN_POINT('Origin',(258.115760998171,-242.,20.));
#25011=CARTESIAN_POINT('Origin',(263.115760998171,-202.,20.));
#25012=CARTESIAN_POINT('',(263.115760998171,-199.5,20.));
#25013=CARTESIAN_POINT('Origin',(263.115760998171,-202.,20.));
#25014=CARTESIAN_POINT('',(258.115760998171,-199.5,20.));
#25015=CARTESIAN_POINT('',(263.115760998171,-199.5,20.));
#25016=CARTESIAN_POINT('Origin',(258.115760998171,-202.,20.));
#25017=CARTESIAN_POINT('Origin',(263.115760998171,-202.,-20.));
#25018=CARTESIAN_POINT('',(263.115760998171,-199.5,-20.));
#25019=CARTESIAN_POINT('Origin',(263.115760998171,-202.,-20.));
#25020=CARTESIAN_POINT('',(258.115760998171,-199.5,-20.));
#25021=CARTESIAN_POINT('',(263.115760998171,-199.5,-20.));
#25022=CARTESIAN_POINT('Origin',(258.115760998171,-202.,-20.));
#25023=CARTESIAN_POINT('Origin',(263.11576099817,242.,20.));
#25024=CARTESIAN_POINT('',(263.11576099817,244.5,20.));
#25025=CARTESIAN_POINT('Origin',(263.11576099817,242.,20.));
#25026=CARTESIAN_POINT('',(258.11576099817,244.5,20.));
#25027=CARTESIAN_POINT('',(263.11576099817,244.5,20.));
#25028=CARTESIAN_POINT('Origin',(258.11576099817,242.,20.));
#25029=CARTESIAN_POINT('Origin',(263.115760998171,202.,-20.));
#25030=CARTESIAN_POINT('',(263.115760998171,204.5,-20.));
#25031=CARTESIAN_POINT('Origin',(263.115760998171,202.,-20.));
#25032=CARTESIAN_POINT('',(258.115760998171,204.5,-20.));
#25033=CARTESIAN_POINT('',(263.115760998171,204.5,-20.));
#25034=CARTESIAN_POINT('Origin',(258.115760998171,202.,-20.));
#25035=CARTESIAN_POINT('Origin',(263.115760998171,202.,20.));
#25036=CARTESIAN_POINT('',(263.115760998171,204.5,20.));
#25037=CARTESIAN_POINT('Origin',(263.115760998171,202.,20.));
#25038=CARTESIAN_POINT('',(258.115760998171,204.5,20.));
#25039=CARTESIAN_POINT('',(263.115760998171,204.5,20.));
#25040=CARTESIAN_POINT('Origin',(258.115760998171,202.,20.));
#25041=CARTESIAN_POINT('Origin',(263.11576099817,242.,-20.));
#25042=CARTESIAN_POINT('',(263.11576099817,244.5,-20.));
#25043=CARTESIAN_POINT('Origin',(263.11576099817,242.,-20.));
#25044=CARTESIAN_POINT('',(258.11576099817,244.5,-20.));
#25045=CARTESIAN_POINT('',(263.11576099817,244.5,-20.));
#25046=CARTESIAN_POINT('Origin',(258.11576099817,242.,-20.));
#25047=CARTESIAN_POINT('Origin',(258.11576099817,222.,0.));
#25048=CARTESIAN_POINT('',(66.475559418481,241.,2.32682891837986E-15));
#25049=CARTESIAN_POINT('Ctrl Pts',(66.475559418481,241.,6.03683769639929E-15));
#25050=CARTESIAN_POINT('Ctrl Pts',(66.475559418481,241.,-0.818914397616676));
#25051=CARTESIAN_POINT('Ctrl Pts',(66.6828156889532,240.943036471407,-1.66914044272295));
#25052=CARTESIAN_POINT('Ctrl Pts',(67.4158253648335,240.738969075332,-3.23661719250768));
#25053=CARTESIAN_POINT('Ctrl Pts',(67.933482619513,240.59373120234,-3.95788330423287));
#25054=CARTESIAN_POINT('Ctrl Pts',(69.6361378266225,240.108932801212,-5.91638068595454));
#25055=CARTESIAN_POINT('Ctrl Pts',(71.1576540050022,239.665242818586,-7.08907003196721));
#25056=CARTESIAN_POINT('Ctrl Pts',(74.3823681679428,238.684108540751,-9.16276251679134));
#25057=CARTESIAN_POINT('Ctrl Pts',(76.0892097916356,238.145315558933,-10.0574548511805));
#25058=CARTESIAN_POINT('Ctrl Pts',(80.5078069493414,236.701116337081,-12.1466632640978));
#25059=CARTESIAN_POINT('Ctrl Pts',(83.5441791540702,235.651195580973,-13.3041009898948));
#25060=CARTESIAN_POINT('Ctrl Pts',(89.798722524918,233.339463641051,-15.32223219563));
#25061=CARTESIAN_POINT('Ctrl Pts',(93.0181628755071,232.0771819994,-16.1784506413274));
#25062=CARTESIAN_POINT('Ctrl Pts',(99.4647393270101,229.388236379592,-17.5700183736559));
#25063=CARTESIAN_POINT('Ctrl Pts',(102.691654775973,227.961595935903,-18.1038606242188));
#25064=CARTESIAN_POINT('Ctrl Pts',(108.98538364367,225.020557582189,-18.8193152708395));
#25065=CARTESIAN_POINT('Ctrl Pts',(112.052307853074,223.506171165075,-19.));
#25066=CARTESIAN_POINT('Ctrl Pts',(119.299384453378,219.753332518616,-19.));
#25067=CARTESIAN_POINT('Ctrl Pts',(123.97020433053,217.157824280152,-18.593013611366));
#25068=CARTESIAN_POINT('Ctrl Pts',(130.550318589395,213.220888597628,-16.9104681529982));
#25069=CARTESIAN_POINT('Ctrl Pts',(132.673701403444,211.903864145767,-16.1734222030093));
#25070=CARTESIAN_POINT('Ctrl Pts',(136.64657075335,209.363973465165,-14.2773379372075));
#25071=CARTESIAN_POINT('Ctrl Pts',(138.497260071169,208.140453793306,-13.1216968983942));
#25072=CARTESIAN_POINT('Ctrl Pts',(140.914378515077,206.504262153928,-11.0274797072174));
#25073=CARTESIAN_POINT('Ctrl Pts',(141.679048846267,205.980033579842,-10.2626502639426));
#25074=CARTESIAN_POINT('Ctrl Pts',(143.080866831829,205.008762402486,-8.55915648524146));
#25075=CARTESIAN_POINT('Ctrl Pts',(143.717851327755,204.561968106359,-7.62021633376244));
#25076=CARTESIAN_POINT('Ctrl Pts',(144.775897909994,203.814520750128,-5.60723443384186));
#25077=CARTESIAN_POINT('Ctrl Pts',(145.197945099354,203.513339264161,-4.53064652501085));
#25078=CARTESIAN_POINT('Ctrl Pts',(145.767257174916,203.105955734851,-2.30184157443626));
#25079=CARTESIAN_POINT('Ctrl Pts',(145.914358443575,203.,-1.14953772934859));
#25080=CARTESIAN_POINT('Ctrl Pts',(145.914358443575,203.,1.14953772934859));
#25081=CARTESIAN_POINT('Ctrl Pts',(145.767257174916,203.105955734851,2.30184157443626));
#25082=CARTESIAN_POINT('Ctrl Pts',(145.197945099354,203.513339264161,4.53064652501085));
#25083=CARTESIAN_POINT('Ctrl Pts',(144.775897909994,203.814520750128,5.60723443384185));
#25084=CARTESIAN_POINT('Ctrl Pts',(143.717851327755,204.561968106359,7.62021633376245));
#25085=CARTESIAN_POINT('Ctrl Pts',(143.080866831829,205.008762402486,8.55915648524148));
#25086=CARTESIAN_POINT('Ctrl Pts',(141.679048846267,205.980033579842,10.2626502639426));
#25087=CARTESIAN_POINT('Ctrl Pts',(140.914378515077,206.504262153928,11.0274797072174));
#25088=CARTESIAN_POINT('Ctrl Pts',(138.497260071169,208.140453793306,13.1216968983942));
#25089=CARTESIAN_POINT('Ctrl Pts',(136.64657075335,209.363973465165,14.2773379372075));
#25090=CARTESIAN_POINT('Ctrl Pts',(132.673701403444,211.903864145767,16.1734222030093));
#25091=CARTESIAN_POINT('Ctrl Pts',(130.550318589395,213.220888597628,16.9104681529982));
#25092=CARTESIAN_POINT('Ctrl Pts',(123.97020433053,217.157824280152,18.593013611366));
#25093=CARTESIAN_POINT('Ctrl Pts',(119.299384453378,219.753332518616,19.));
#25094=CARTESIAN_POINT('Ctrl Pts',(112.052307853074,223.506171165075,19.));
#25095=CARTESIAN_POINT('Ctrl Pts',(108.98538364367,225.020557582189,18.8193152708395));
#25096=CARTESIAN_POINT('Ctrl Pts',(102.691654775973,227.961595935903,18.1038606242188));
#25097=CARTESIAN_POINT('Ctrl Pts',(99.4647393270101,229.388236379592,17.5700183736559));
#25098=CARTESIAN_POINT('Ctrl Pts',(93.0181628755072,232.0771819994,16.1784506413274));
#25099=CARTESIAN_POINT('Ctrl Pts',(89.798722524918,233.339463641051,15.32223219563));
#25100=CARTESIAN_POINT('Ctrl Pts',(83.5441791540702,235.651195580973,13.3041009898948));
#25101=CARTESIAN_POINT('Ctrl Pts',(80.5078069493414,236.701116337081,12.1466632640978));
#25102=CARTESIAN_POINT('Ctrl Pts',(76.0892097916356,238.145315558933,10.0574548511805));
#25103=CARTESIAN_POINT('Ctrl Pts',(74.3823681679427,238.684108540751,9.16276251679135));
#25104=CARTESIAN_POINT('Ctrl Pts',(71.1576540050022,239.665242818586,7.08907003196723));
#25105=CARTESIAN_POINT('Ctrl Pts',(69.6361378266225,240.108932801212,5.91638068595453));
#25106=CARTESIAN_POINT('Ctrl Pts',(67.933482619513,240.59373120234,3.95788330423286));
#25107=CARTESIAN_POINT('Ctrl Pts',(67.4158253648334,240.738969075332,3.23661719250768));
#25108=CARTESIAN_POINT('Ctrl Pts',(66.6828156889532,240.943036471406,1.66914044272293));
#25109=CARTESIAN_POINT('Ctrl Pts',(66.475559418481,241.,0.818914397616675));
#25110=CARTESIAN_POINT('Ctrl Pts',(66.475559418481,241.,-8.32667268468867E-16));
#25111=CARTESIAN_POINT('',(258.11576099817,241.,-2.32682891837997E-15));
#25112=CARTESIAN_POINT('',(258.11576099817,241.,-2.32682891837997E-15));
#25113=CARTESIAN_POINT('Origin',(258.11576099817,222.,0.));
#25114=CARTESIAN_POINT('Origin',(258.115760998171,-222.,0.));
#25115=CARTESIAN_POINT('',(145.914358443575,-203.,0.));
#25116=CARTESIAN_POINT('Ctrl Pts',(145.914358443575,-203.,1.94289029309402E-15));
#25117=CARTESIAN_POINT('Ctrl Pts',(145.914358443575,-203.,-1.14953772934859));
#25118=CARTESIAN_POINT('Ctrl Pts',(145.767257174916,-203.105955734851,-2.30184157443626));
#25119=CARTESIAN_POINT('Ctrl Pts',(145.197945099354,-203.513339264161,-4.53064652501085));
#25120=CARTESIAN_POINT('Ctrl Pts',(144.775897909994,-203.814520750128,-5.60723443384187));
#25121=CARTESIAN_POINT('Ctrl Pts',(143.717851327755,-204.561968106359,-7.62021633376246));
#25122=CARTESIAN_POINT('Ctrl Pts',(143.080866831829,-205.008762402486,-8.55915648524147));
#25123=CARTESIAN_POINT('Ctrl Pts',(141.679048846267,-205.980033579842,-10.2626502639426));
#25124=CARTESIAN_POINT('Ctrl Pts',(140.914378515077,-206.504262153928,-11.0274797072174));
#25125=CARTESIAN_POINT('Ctrl Pts',(138.497260071169,-208.140453793306,-13.1216968983942));
#25126=CARTESIAN_POINT('Ctrl Pts',(136.64657075335,-209.363973465165,-14.2773379372076));
#25127=CARTESIAN_POINT('Ctrl Pts',(132.673701403444,-211.903864145766,-16.1734222030094));
#25128=CARTESIAN_POINT('Ctrl Pts',(130.550318589395,-213.220888597628,-16.9104681529982));
#25129=CARTESIAN_POINT('Ctrl Pts',(123.97020433053,-217.157824280152,-18.593013611366));
#25130=CARTESIAN_POINT('Ctrl Pts',(119.299384453378,-219.753332518616,-19.));
#25131=CARTESIAN_POINT('Ctrl Pts',(112.052307853074,-223.506171165075,-19.));
#25132=CARTESIAN_POINT('Ctrl Pts',(108.98538364367,-225.020557582189,-18.8193152708395));
#25133=CARTESIAN_POINT('Ctrl Pts',(102.691654775973,-227.961595935903,-18.1038606242189));
#25134=CARTESIAN_POINT('Ctrl Pts',(99.46473932701,-229.388236379592,-17.570018373656));
#25135=CARTESIAN_POINT('Ctrl Pts',(93.0181628755071,-232.0771819994,-16.1784506413275));
#25136=CARTESIAN_POINT('Ctrl Pts',(89.7987225249179,-233.339463641051,-15.32223219563));
#25137=CARTESIAN_POINT('Ctrl Pts',(83.5441791540701,-235.651195580973,-13.3041009898948));
#25138=CARTESIAN_POINT('Ctrl Pts',(80.5078069493413,-236.701116337082,-12.1466632640978));
#25139=CARTESIAN_POINT('Ctrl Pts',(76.0892097916354,-238.145315558933,-10.0574548511805));
#25140=CARTESIAN_POINT('Ctrl Pts',(74.3823681679425,-238.684108540751,-9.16276251679143));
#25141=CARTESIAN_POINT('Ctrl Pts',(71.157654005002,-239.665242818586,-7.08907003196732));
#25142=CARTESIAN_POINT('Ctrl Pts',(69.6361378266224,-240.108932801212,-5.91638068595454));
#25143=CARTESIAN_POINT('Ctrl Pts',(67.9334826195128,-240.593731202341,-3.95788330423287));
#25144=CARTESIAN_POINT('Ctrl Pts',(67.4158253648332,-240.738969075332,-3.23661719250773));
#25145=CARTESIAN_POINT('Ctrl Pts',(66.6828156889529,-240.943036471407,-1.669140442723));
#25146=CARTESIAN_POINT('Ctrl Pts',(66.4755594184807,-241.,-0.818914397616677));
#25147=CARTESIAN_POINT('Ctrl Pts',(66.4755594184807,-241.,0.818914397616677));
#25148=CARTESIAN_POINT('Ctrl Pts',(66.6828156889529,-240.943036471407,1.669140442723));
#25149=CARTESIAN_POINT('Ctrl Pts',(67.4158253648332,-240.738969075332,3.23661719250773));
#25150=CARTESIAN_POINT('Ctrl Pts',(67.9334826195128,-240.593731202341,3.95788330423287));
#25151=CARTESIAN_POINT('Ctrl Pts',(69.6361378266224,-240.108932801212,5.91638068595454));
#25152=CARTESIAN_POINT('Ctrl Pts',(71.157654005002,-239.665242818586,7.0890700319673));
#25153=CARTESIAN_POINT('Ctrl Pts',(74.3823681679425,-238.684108540751,9.1627625167914));
#25154=CARTESIAN_POINT('Ctrl Pts',(76.0892097916354,-238.145315558933,10.0574548511805));
#25155=CARTESIAN_POINT('Ctrl Pts',(80.5078069493413,-236.701116337082,12.1466632640978));
#25156=CARTESIAN_POINT('Ctrl Pts',(83.5441791540701,-235.651195580973,13.3041009898948));
#25157=CARTESIAN_POINT('Ctrl Pts',(89.7987225249179,-233.339463641051,15.32223219563));
#25158=CARTESIAN_POINT('Ctrl Pts',(93.0181628755071,-232.0771819994,16.1784506413275));
#25159=CARTESIAN_POINT('Ctrl Pts',(99.46473932701,-229.388236379592,17.570018373656));
#25160=CARTESIAN_POINT('Ctrl Pts',(102.691654775973,-227.961595935903,18.1038606242189));
#25161=CARTESIAN_POINT('Ctrl Pts',(108.98538364367,-225.020557582189,18.8193152708395));
#25162=CARTESIAN_POINT('Ctrl Pts',(112.052307853074,-223.506171165075,19.));
#25163=CARTESIAN_POINT('Ctrl Pts',(119.299384453378,-219.753332518616,19.));
#25164=CARTESIAN_POINT('Ctrl Pts',(123.97020433053,-217.157824280152,18.593013611366));
#25165=CARTESIAN_POINT('Ctrl Pts',(130.550318589395,-213.220888597628,16.9104681529982));
#25166=CARTESIAN_POINT('Ctrl Pts',(132.673701403444,-211.903864145766,16.1734222030093));
#25167=CARTESIAN_POINT('Ctrl Pts',(136.64657075335,-209.363973465165,14.2773379372076));
#25168=CARTESIAN_POINT('Ctrl Pts',(138.497260071169,-208.140453793306,13.1216968983942));
#25169=CARTESIAN_POINT('Ctrl Pts',(140.914378515077,-206.504262153928,11.0274797072174));
#25170=CARTESIAN_POINT('Ctrl Pts',(141.679048846267,-205.980033579842,10.2626502639426));
#25171=CARTESIAN_POINT('Ctrl Pts',(143.080866831829,-205.008762402486,8.55915648524147));
#25172=CARTESIAN_POINT('Ctrl Pts',(143.717851327756,-204.561968106359,7.62021633376245));
#25173=CARTESIAN_POINT('Ctrl Pts',(144.775897909994,-203.814520750128,5.60723443384185));
#25174=CARTESIAN_POINT('Ctrl Pts',(145.197945099354,-203.513339264161,4.53064652501084));
#25175=CARTESIAN_POINT('Ctrl Pts',(145.767257174916,-203.105955734851,2.30184157443625));
#25176=CARTESIAN_POINT('Ctrl Pts',(145.914358443575,-203.,1.14953772934859));
#25177=CARTESIAN_POINT('Ctrl Pts',(145.914358443575,-203.,-5.55111512312578E-16));
#25178=CARTESIAN_POINT('',(258.115760998171,-203.,-2.32682891837997E-15));
#25179=CARTESIAN_POINT('',(258.115760998171,-203.,-2.32682891837997E-15));
#25180=CARTESIAN_POINT('Origin',(258.115760998171,-222.,0.));
#25181=CARTESIAN_POINT('Origin',(163.11576099817,-222.,0.));
#25182=CARTESIAN_POINT('',(121.453694879983,-207.,-1.8369702010623E-15));
#25183=CARTESIAN_POINT('Ctrl Pts',(121.453694879983,-207.,5.55111512312578E-16));
#25184=CARTESIAN_POINT('Ctrl Pts',(121.453694879983,-207.,0.907353133092068));
#25185=CARTESIAN_POINT('Ctrl Pts',(121.312112526369,-207.083231650701,1.80198099765884));
#25186=CARTESIAN_POINT('Ctrl Pts',(120.784107112644,-207.391641455618,3.5146797882098));
#25187=CARTESIAN_POINT('Ctrl Pts',(120.397755245695,-207.616671164825,4.33279938877936));
#25188=CARTESIAN_POINT('Ctrl Pts',(118.970528778436,-208.439967174701,6.61351349009191));
#25189=CARTESIAN_POINT('Ctrl Pts',(117.651916050567,-209.18968749672,7.90128916914638));
#25190=CARTESIAN_POINT('Ctrl Pts',(114.642831125276,-210.85711562393,10.1640207575769));
#25191=CARTESIAN_POINT('Ctrl Pts',(112.759779424709,-211.873400908832,11.1431178977762));
#25192=CARTESIAN_POINT('Ctrl Pts',(108.75053729299,-213.958936505348,12.7302152622124));
#25193=CARTESIAN_POINT('Ctrl Pts',(106.622299465224,-215.02926865615,13.3316141536719));
#25194=CARTESIAN_POINT('Ctrl Pts',(100.060775208621,-218.200471522578,14.6920280995398));
#25195=CARTESIAN_POINT('Ctrl Pts',(95.4525107000109,-220.249930762303,15.));
#25196=CARTESIAN_POINT('Ctrl Pts',(88.0210425552756,-223.302593927956,15.));
#25197=CARTESIAN_POINT('Ctrl Pts',(84.6790306087128,-224.594675453913,14.8289890919114));
#25198=CARTESIAN_POINT('Ctrl Pts',(77.8141827696673,-227.064438929898,14.1768373375443));
#25199=CARTESIAN_POINT('Ctrl Pts',(74.2912554085806,-228.242073248777,13.6964791866782));
#25200=CARTESIAN_POINT('Ctrl Pts',(67.2345931481628,-230.419495002038,12.4767593682344));
#25201=CARTESIAN_POINT('Ctrl Pts',(63.7008186732762,-231.41933527847,11.7385985584428));
#25202=CARTESIAN_POINT('Ctrl Pts',(56.8008352730486,-233.208850905064,10.0439158689026));
#25203=CARTESIAN_POINT('Ctrl Pts',(53.4336788142811,-233.998786023356,9.09152888694572));
#25204=CARTESIAN_POINT('Ctrl Pts',(48.5152345428215,-235.051962812042,7.4250013775077));
#25205=CARTESIAN_POINT('Ctrl Pts',(46.6209703458263,-235.43570474664,6.72770406164338));
#25206=CARTESIAN_POINT('Ctrl Pts',(43.8696416840566,-235.958313851502,5.51005073346341));
#25207=CARTESIAN_POINT('Ctrl Pts',(42.9682669434626,-236.123872251653,5.075737390253));
#25208=CARTESIAN_POINT('Ctrl Pts',(41.2574066533486,-236.428808311227,4.12993654891045));
#25209=CARTESIAN_POINT('Ctrl Pts',(40.4462113162161,-236.568461801527,3.62163429304668));
#25210=CARTESIAN_POINT('Ctrl Pts',(39.2605592418267,-236.767462602177,2.65913427303629));
#25211=CARTESIAN_POINT('Ctrl Pts',(38.7825283359309,-236.846042324477,2.20487590415701));
#25212=CARTESIAN_POINT('Ctrl Pts',(38.2440350776008,-236.933380610508,1.43553363474373));
#25213=CARTESIAN_POINT('Ctrl Pts',(38.0943087821406,-236.957453393979,1.16408998649961));
#25214=CARTESIAN_POINT('Ctrl Pts',(37.8864347500152,-236.990778602197,0.597557056254765));
#25215=CARTESIAN_POINT('Ctrl Pts',(37.8285606387555,-237.,0.302365587737163));
#25216=CARTESIAN_POINT('Ctrl Pts',(37.8285606387555,-237.,-0.302365587737163));
#25217=CARTESIAN_POINT('Ctrl Pts',(37.8864347500152,-236.990778602197,-0.597557056254765));
#25218=CARTESIAN_POINT('Ctrl Pts',(38.0943087821406,-236.957453393979,-1.16408998649961));
#25219=CARTESIAN_POINT('Ctrl Pts',(38.2440350776008,-236.933380610508,-1.43553363474373));
#25220=CARTESIAN_POINT('Ctrl Pts',(38.7825283359309,-236.846042324477,-2.20487590415701));
#25221=CARTESIAN_POINT('Ctrl Pts',(39.2605592418267,-236.767462602177,-2.65913427303629));
#25222=CARTESIAN_POINT('Ctrl Pts',(40.4462113162161,-236.568461801527,-3.62163429304668));
#25223=CARTESIAN_POINT('Ctrl Pts',(41.2574066533486,-236.428808311227,-4.12993654891045));
#25224=CARTESIAN_POINT('Ctrl Pts',(42.9682669434626,-236.123872251653,-5.075737390253));
#25225=CARTESIAN_POINT('Ctrl Pts',(43.8696416840566,-235.958313851502,-5.51005073346341));
#25226=CARTESIAN_POINT('Ctrl Pts',(46.6209703458263,-235.43570474664,-6.72770406164338));
#25227=CARTESIAN_POINT('Ctrl Pts',(48.5152345428215,-235.051962812042,-7.4250013775077));
#25228=CARTESIAN_POINT('Ctrl Pts',(53.4336788142811,-233.998786023356,-9.09152888694572));
#25229=CARTESIAN_POINT('Ctrl Pts',(56.8008352730486,-233.208850905064,-10.0439158689026));
#25230=CARTESIAN_POINT('Ctrl Pts',(63.7008186732762,-231.41933527847,-11.7385985584428));
#25231=CARTESIAN_POINT('Ctrl Pts',(67.2345931481628,-230.419495002038,-12.4767593682344));
#25232=CARTESIAN_POINT('Ctrl Pts',(74.2912554085806,-228.242073248777,-13.6964791866782));
#25233=CARTESIAN_POINT('Ctrl Pts',(77.8141827696673,-227.064438929898,-14.1768373375443));
#25234=CARTESIAN_POINT('Ctrl Pts',(84.6790306087128,-224.594675453913,-14.8289890919114));
#25235=CARTESIAN_POINT('Ctrl Pts',(88.0210425552756,-223.302593927956,-15.));
#25236=CARTESIAN_POINT('Ctrl Pts',(95.4525107000109,-220.249930762303,-15.));
#25237=CARTESIAN_POINT('Ctrl Pts',(100.060775208621,-218.200471522578,-14.6920280995398));
#25238=CARTESIAN_POINT('Ctrl Pts',(106.622299465224,-215.02926865615,-13.3316141536719));
#25239=CARTESIAN_POINT('Ctrl Pts',(108.75053729299,-213.958936505348,-12.7302152622124));
#25240=CARTESIAN_POINT('Ctrl Pts',(112.759779424709,-211.873400908832,-11.1431178977762));
#25241=CARTESIAN_POINT('Ctrl Pts',(114.642831125276,-210.85711562393,-10.1640207575769));
#25242=CARTESIAN_POINT('Ctrl Pts',(117.651916050567,-209.18968749672,-7.90128916914638));
#25243=CARTESIAN_POINT('Ctrl Pts',(118.970528778436,-208.439967174701,-6.61351349009191));
#25244=CARTESIAN_POINT('Ctrl Pts',(120.397755245695,-207.616671164825,-4.33279938877936));
#25245=CARTESIAN_POINT('Ctrl Pts',(120.784107112644,-207.391641455618,-3.5146797882098));
#25246=CARTESIAN_POINT('Ctrl Pts',(121.312112526369,-207.083231650701,-1.80198099765884));
#25247=CARTESIAN_POINT('Ctrl Pts',(121.453694879983,-207.,-0.907353133092065));
#25248=CARTESIAN_POINT('Ctrl Pts',(121.453694879983,-207.,2.77555756156289E-15));
#25249=CARTESIAN_POINT('',(263.115760998171,-207.,1.83697019872103E-15));
#25250=CARTESIAN_POINT('',(163.11576099817,-207.,1.83697019872103E-15));
#25251=CARTESIAN_POINT('Origin',(263.115760998171,-222.,0.));
#25252=CARTESIAN_POINT('Origin',(163.11576099817,222.,0.));
#25253=CARTESIAN_POINT('',(121.453694879983,207.,1.8369702010623E-15));
#25254=CARTESIAN_POINT('Ctrl Pts',(37.8285606387552,237.,6.76542155630955E-15));
#25255=CARTESIAN_POINT('Ctrl Pts',(37.8285606387552,237.,0.302365587737165));
#25256=CARTESIAN_POINT('Ctrl Pts',(37.8864347500152,236.990778602197,0.59755705625476));
#25257=CARTESIAN_POINT('Ctrl Pts',(38.0943087821406,236.957453393979,1.16408998649961));
#25258=CARTESIAN_POINT('Ctrl Pts',(38.2440350776008,236.933380610508,1.43553363474373));
#25259=CARTESIAN_POINT('Ctrl Pts',(38.7825283359309,236.846042324477,2.20487590415701));
#25260=CARTESIAN_POINT('Ctrl Pts',(39.2605592418267,236.767462602177,2.65913427303628));
#25261=CARTESIAN_POINT('Ctrl Pts',(40.4462113162161,236.568461801527,3.62163429304667));
#25262=CARTESIAN_POINT('Ctrl Pts',(41.2574066533486,236.428808311227,4.12993654891044));
#25263=CARTESIAN_POINT('Ctrl Pts',(42.9682669434626,236.123872251653,5.07573739025299));
#25264=CARTESIAN_POINT('Ctrl Pts',(43.8696416840566,235.958313851502,5.51005073346341));
#25265=CARTESIAN_POINT('Ctrl Pts',(46.6209703458263,235.43570474664,6.72770406164338));
#25266=CARTESIAN_POINT('Ctrl Pts',(48.5152345428215,235.051962812042,7.4250013775077));
#25267=CARTESIAN_POINT('Ctrl Pts',(53.4336788142811,233.998786023356,9.09152888694572));
#25268=CARTESIAN_POINT('Ctrl Pts',(56.8008352730486,233.208850905064,10.0439158689026));
#25269=CARTESIAN_POINT('Ctrl Pts',(63.7008186732762,231.41933527847,11.7385985584428));
#25270=CARTESIAN_POINT('Ctrl Pts',(67.2345931481628,230.419495002039,12.4767593682344));
#25271=CARTESIAN_POINT('Ctrl Pts',(74.2912554085806,228.242073248777,13.6964791866782));
#25272=CARTESIAN_POINT('Ctrl Pts',(77.8141827696673,227.064438929898,14.1768373375443));
#25273=CARTESIAN_POINT('Ctrl Pts',(84.6790306087128,224.594675453913,14.8289890919114));
#25274=CARTESIAN_POINT('Ctrl Pts',(88.0210425552756,223.302593927956,15.));
#25275=CARTESIAN_POINT('Ctrl Pts',(95.4525107000109,220.249930762303,15.));
#25276=CARTESIAN_POINT('Ctrl Pts',(100.060775208621,218.200471522578,14.6920280995398));
#25277=CARTESIAN_POINT('Ctrl Pts',(106.622299465224,215.02926865615,13.3316141536719));
#25278=CARTESIAN_POINT('Ctrl Pts',(108.75053729299,213.958936505348,12.7302152622124));
#25279=CARTESIAN_POINT('Ctrl Pts',(112.759779424709,211.873400908832,11.1431178977762));
#25280=CARTESIAN_POINT('Ctrl Pts',(114.642831125276,210.85711562393,10.1640207575769));
#25281=CARTESIAN_POINT('Ctrl Pts',(117.651916050567,209.18968749672,7.90128916914638));
#25282=CARTESIAN_POINT('Ctrl Pts',(118.970528778436,208.439967174701,6.6135134900919));
#25283=CARTESIAN_POINT('Ctrl Pts',(120.397755245695,207.616671164825,4.33279938877936));
#25284=CARTESIAN_POINT('Ctrl Pts',(120.784107112644,207.391641455618,3.5146797882098));
#25285=CARTESIAN_POINT('Ctrl Pts',(121.312112526369,207.083231650701,1.80198099765883));
#25286=CARTESIAN_POINT('Ctrl Pts',(121.453694879983,207.,0.907353133092066));
#25287=CARTESIAN_POINT('Ctrl Pts',(121.453694879983,207.,-0.907353133092066));
#25288=CARTESIAN_POINT('Ctrl Pts',(121.312112526369,207.083231650701,-1.80198099765884));
#25289=CARTESIAN_POINT('Ctrl Pts',(120.784107112644,207.391641455618,-3.5146797882098));
#25290=CARTESIAN_POINT('Ctrl Pts',(120.397755245695,207.616671164825,-4.33279938877936));
#25291=CARTESIAN_POINT('Ctrl Pts',(118.970528778436,208.439967174701,-6.6135134900919));
#25292=CARTESIAN_POINT('Ctrl Pts',(117.651916050567,209.18968749672,-7.90128916914638));
#25293=CARTESIAN_POINT('Ctrl Pts',(114.642831125276,210.85711562393,-10.1640207575769));
#25294=CARTESIAN_POINT('Ctrl Pts',(112.759779424709,211.873400908832,-11.1431178977762));
#25295=CARTESIAN_POINT('Ctrl Pts',(108.75053729299,213.958936505348,-12.7302152622124));
#25296=CARTESIAN_POINT('Ctrl Pts',(106.622299465224,215.02926865615,-13.3316141536719));
#25297=CARTESIAN_POINT('Ctrl Pts',(100.060775208621,218.200471522578,-14.6920280995398));
#25298=CARTESIAN_POINT('Ctrl Pts',(95.4525107000109,220.249930762303,-15.));
#25299=CARTESIAN_POINT('Ctrl Pts',(88.0210425552756,223.302593927956,-15.));
#25300=CARTESIAN_POINT('Ctrl Pts',(84.6790306087128,224.594675453913,-14.8289890919114));
#25301=CARTESIAN_POINT('Ctrl Pts',(77.8141827696673,227.064438929898,-14.1768373375443));
#25302=CARTESIAN_POINT('Ctrl Pts',(74.2912554085806,228.242073248777,-13.6964791866782));
#25303=CARTESIAN_POINT('Ctrl Pts',(67.2345931481628,230.419495002038,-12.4767593682344));
#25304=CARTESIAN_POINT('Ctrl Pts',(63.7008186732762,231.41933527847,-11.7385985584428));
#25305=CARTESIAN_POINT('Ctrl Pts',(56.8008352730486,233.208850905064,-10.0439158689026));
#25306=CARTESIAN_POINT('Ctrl Pts',(53.4336788142811,233.998786023356,-9.09152888694572));
#25307=CARTESIAN_POINT('Ctrl Pts',(48.5152345428215,235.051962812042,-7.4250013775077));
#25308=CARTESIAN_POINT('Ctrl Pts',(46.6209703458263,235.43570474664,-6.72770406164338));
#25309=CARTESIAN_POINT('Ctrl Pts',(43.8696416840566,235.958313851502,-5.51005073346341));
#25310=CARTESIAN_POINT('Ctrl Pts',(42.9682669434626,236.123872251653,-5.07573739025299));
#25311=CARTESIAN_POINT('Ctrl Pts',(41.2574066533486,236.428808311227,-4.12993654891044));
#25312=CARTESIAN_POINT('Ctrl Pts',(40.4462113162161,236.568461801527,-3.62163429304667));
#25313=CARTESIAN_POINT('Ctrl Pts',(39.2605592418267,236.767462602177,-2.65913427303628));
#25314=CARTESIAN_POINT('Ctrl Pts',(38.7825283359309,236.846042324477,-2.20487590415701));
#25315=CARTESIAN_POINT('Ctrl Pts',(38.2440350776008,236.933380610508,-1.43553363474373));
#25316=CARTESIAN_POINT('Ctrl Pts',(38.0943087821406,236.957453393979,-1.16408998649961));
#25317=CARTESIAN_POINT('Ctrl Pts',(37.8864347500152,236.990778602197,-0.597557056254762));
#25318=CARTESIAN_POINT('Ctrl Pts',(37.8285606387552,237.,-0.302365587737161));
#25319=CARTESIAN_POINT('Ctrl Pts',(37.8285606387552,237.,0.));
#25320=CARTESIAN_POINT('',(263.11576099817,207.,-1.83697019872103E-15));
#25321=CARTESIAN_POINT('',(163.11576099817,207.,-1.83697019872103E-15));
#25322=CARTESIAN_POINT('Origin',(263.11576099817,222.,0.));
#25323=CARTESIAN_POINT('Origin',(0.,0.,-65.));
#25324=CARTESIAN_POINT('',(-25.,-3.06161699786838E-15,-35.));
#25325=CARTESIAN_POINT('',(-25.,-3.06161699786838E-15,-65.));
#25326=CARTESIAN_POINT('Origin',(0.,0.,-35.));
#25327=CARTESIAN_POINT('Origin',(0.,267.,35.));
#25328=CARTESIAN_POINT('',(-2.5,267.,45.));
#25329=CARTESIAN_POINT('Origin',(0.,267.,45.));
#25330=CARTESIAN_POINT('',(-2.5,267.,55.));
#25331=CARTESIAN_POINT('',(-2.5,267.,35.));
#25332=CARTESIAN_POINT('Origin',(0.,267.,55.));
#25333=CARTESIAN_POINT('Origin',(108.598683701239,243.916637190574,35.));
#25334=CARTESIAN_POINT('',(106.098683701239,243.916637190574,45.));
#25335=CARTESIAN_POINT('Origin',(108.598683701239,243.916637190574,45.));
#25336=CARTESIAN_POINT('',(106.098683701239,243.916637190574,55.));
#25337=CARTESIAN_POINT('',(106.098683701239,243.916637190574,35.));
#25338=CARTESIAN_POINT('Origin',(108.598683701239,243.916637190574,55.));
#25339=CARTESIAN_POINT('Origin',(198.419668402464,178.657871897815,35.));
#25340=CARTESIAN_POINT('',(195.919668402464,178.657871897815,45.));
#25341=CARTESIAN_POINT('Origin',(198.419668402464,178.657871897815,45.));
#25342=CARTESIAN_POINT('',(195.919668402464,178.657871897815,55.));
#25343=CARTESIAN_POINT('',(195.919668402464,178.657871897815,35.));
#25344=CARTESIAN_POINT('Origin',(198.419668402464,178.657871897815,55.));
#25345=CARTESIAN_POINT('Origin',(253.932089850806,82.507537498111,35.));
#25346=CARTESIAN_POINT('',(251.432089850806,82.507537498111,45.));
#25347=CARTESIAN_POINT('Origin',(253.932089850806,82.507537498111,45.));
#25348=CARTESIAN_POINT('',(251.432089850806,82.507537498111,55.));
#25349=CARTESIAN_POINT('',(251.432089850806,82.507537498111,35.));
#25350=CARTESIAN_POINT('Origin',(253.932089850806,82.507537498111,55.));
#25351=CARTESIAN_POINT('Origin',(265.537346063329,-27.9090996924634,35.));
#25352=CARTESIAN_POINT('',(263.037346063329,-27.9090996924634,45.));
#25353=CARTESIAN_POINT('Origin',(265.537346063329,-27.9090996924634,45.));
#25354=CARTESIAN_POINT('',(263.037346063329,-27.9090996924634,55.));
#25355=CARTESIAN_POINT('',(263.037346063329,-27.9090996924634,35.));
#25356=CARTESIAN_POINT('Origin',(265.537346063329,-27.9090996924634,55.));
#25357=CARTESIAN_POINT('Origin',(231.228782810445,-133.5,35.));
#25358=CARTESIAN_POINT('',(228.728782810445,-133.5,45.));
#25359=CARTESIAN_POINT('Origin',(231.228782810445,-133.5,45.));
#25360=CARTESIAN_POINT('',(228.728782810445,-133.5,55.));
#25361=CARTESIAN_POINT('',(228.728782810445,-133.5,35.));
#25362=CARTESIAN_POINT('Origin',(231.228782810445,-133.5,55.));
#25363=CARTESIAN_POINT('Origin',(156.93866236209,-216.007537498111,35.));
#25364=CARTESIAN_POINT('',(154.43866236209,-216.007537498111,45.));
#25365=CARTESIAN_POINT('Origin',(156.93866236209,-216.007537498111,45.));
#25366=CARTESIAN_POINT('',(154.43866236209,-216.007537498111,55.));
#25367=CARTESIAN_POINT('',(154.43866236209,-216.007537498111,35.));
#25368=CARTESIAN_POINT('Origin',(156.93866236209,-216.007537498111,55.));
#25369=CARTESIAN_POINT('Origin',(55.5124214483419,-261.165409395926,35.));
#25370=CARTESIAN_POINT('',(53.0124214483419,-261.165409395926,45.));
#25371=CARTESIAN_POINT('Origin',(55.5124214483419,-261.165409395926,45.));
#25372=CARTESIAN_POINT('',(53.0124214483419,-261.165409395926,55.));
#25373=CARTESIAN_POINT('',(53.0124214483419,-261.165409395926,35.));
#25374=CARTESIAN_POINT('Origin',(55.5124214483419,-261.165409395926,55.));
#25375=CARTESIAN_POINT('Origin',(-55.5124214483417,-261.165409395926,35.));
#25376=CARTESIAN_POINT('',(-58.0124214483417,-261.165409395926,45.));
#25377=CARTESIAN_POINT('Origin',(-55.5124214483417,-261.165409395926,45.));
#25378=CARTESIAN_POINT('',(-58.0124214483417,-261.165409395926,55.));
#25379=CARTESIAN_POINT('',(-58.0124214483417,-261.165409395926,35.));
#25380=CARTESIAN_POINT('Origin',(-55.5124214483417,-261.165409395926,55.));
#25381=CARTESIAN_POINT('Origin',(-156.93866236209,-216.007537498111,35.));
#25382=CARTESIAN_POINT('',(-159.43866236209,-216.007537498111,45.));
#25383=CARTESIAN_POINT('Origin',(-156.93866236209,-216.007537498111,45.));
#25384=CARTESIAN_POINT('',(-159.43866236209,-216.007537498111,55.));
#25385=CARTESIAN_POINT('',(-159.43866236209,-216.007537498111,35.));
#25386=CARTESIAN_POINT('Origin',(-156.93866236209,-216.007537498111,55.));
#25387=CARTESIAN_POINT('Origin',(-231.228782810445,-133.5,35.));
#25388=CARTESIAN_POINT('',(-233.728782810445,-133.5,45.));
#25389=CARTESIAN_POINT('Origin',(-231.228782810445,-133.5,45.));
#25390=CARTESIAN_POINT('',(-233.728782810445,-133.5,55.));
#25391=CARTESIAN_POINT('',(-233.728782810445,-133.5,35.));
#25392=CARTESIAN_POINT('Origin',(-231.228782810445,-133.5,55.));
#25393=CARTESIAN_POINT('Origin',(-265.537346063329,-27.9090996924637,35.));
#25394=CARTESIAN_POINT('',(-268.037346063329,-27.9090996924637,45.));
#25395=CARTESIAN_POINT('Origin',(-265.537346063329,-27.9090996924637,45.));
#25396=CARTESIAN_POINT('',(-268.037346063329,-27.9090996924637,55.));
#25397=CARTESIAN_POINT('',(-268.037346063329,-27.9090996924637,35.));
#25398=CARTESIAN_POINT('Origin',(-265.537346063329,-27.9090996924637,55.));
#25399=CARTESIAN_POINT('Origin',(-253.932089850806,82.5075374981109,35.));
#25400=CARTESIAN_POINT('',(-256.432089850806,82.5075374981109,45.));
#25401=CARTESIAN_POINT('Origin',(-253.932089850806,82.5075374981109,45.));
#25402=CARTESIAN_POINT('',(-256.432089850806,82.5075374981109,55.));
#25403=CARTESIAN_POINT('',(-256.432089850806,82.5075374981109,35.));
#25404=CARTESIAN_POINT('Origin',(-253.932089850806,82.5075374981109,55.));
#25405=CARTESIAN_POINT('Origin',(-198.419668402464,178.657871897815,35.));
#25406=CARTESIAN_POINT('',(-200.919668402464,178.657871897815,45.));
#25407=CARTESIAN_POINT('Origin',(-198.419668402464,178.657871897815,45.));
#25408=CARTESIAN_POINT('',(-200.919668402464,178.657871897815,55.));
#25409=CARTESIAN_POINT('',(-200.919668402464,178.657871897815,35.));
#25410=CARTESIAN_POINT('Origin',(-198.419668402464,178.657871897815,55.));
#25411=CARTESIAN_POINT('Origin',(-108.598683701239,243.916637190575,35.));
#25412=CARTESIAN_POINT('',(-111.098683701239,243.916637190575,45.));
#25413=CARTESIAN_POINT('Origin',(-108.598683701239,243.916637190575,45.));
#25414=CARTESIAN_POINT('',(-111.098683701239,243.916637190575,55.));
#25415=CARTESIAN_POINT('',(-111.098683701239,243.916637190575,35.));
#25416=CARTESIAN_POINT('Origin',(-108.598683701239,243.916637190575,55.));
#25417=CARTESIAN_POINT('Origin',(0.,0.,55.));
#25418=CARTESIAN_POINT('',(250.,-3.06161699786838E-14,45.));
#25419=CARTESIAN_POINT('',(250.,-3.06161699786838E-14,55.));
#25420=CARTESIAN_POINT('Origin',(0.,0.,45.));
#25421=CARTESIAN_POINT('Origin',(0.,0.,45.));
#25422=CARTESIAN_POINT('',(-275.,-3.36777869765522E-14,55.));
#25423=CARTESIAN_POINT('Origin',(0.,0.,55.));
#25424=CARTESIAN_POINT('',(-275.,-3.36777869765522E-14,45.));
#25425=CARTESIAN_POINT('',(-275.,-3.36777869765522E-14,45.));
#25426=CARTESIAN_POINT('Origin',(0.,0.,45.));
#25427=CARTESIAN_POINT('Origin',(0.,0.,-733.822509939086));
#25428=CARTESIAN_POINT('',(-240.,-2.93915231795365E-14,-45.));
#25429=CARTESIAN_POINT('Origin',(0.,0.,-45.));
#25430=CARTESIAN_POINT('',(-240.,-2.93915231795365E-14,55.));
#25431=CARTESIAN_POINT('',(-240.,-2.93915231795365E-14,-733.822509939086));
#25432=CARTESIAN_POINT('Origin',(0.,0.,55.));
#25433=CARTESIAN_POINT('Origin',(0.,0.,-45.));
#25434=CARTESIAN_POINT('',(42.0243552790815,46.1933668131508,-45.));
#25435=CARTESIAN_POINT('',(42.0243552790815,46.193366813151,-45.));
#25436=CARTESIAN_POINT('',(61.0168067860623,13.2974758427732,-45.));
#25437=CARTESIAN_POINT('',(61.0168067860623,13.2974758427731,-45.));
#25438=CARTESIAN_POINT('',(61.885047674397,8.37343707771113,-45.));
#25439=CARTESIAN_POINT('',(61.885047674397,8.37343707771212,-45.));
#25440=CARTESIAN_POINT('',(61.885047674397,8.37343707771212,-45.));
#25441=CARTESIAN_POINT('',(55.289038487168,-29.0343899078532,-45.));
#25442=CARTESIAN_POINT('',(55.289038487168,-29.0343899078532,-45.));
#25443=CARTESIAN_POINT('',(52.7890384871678,-33.3645169267754,-45.));
#25444=CARTESIAN_POINT('',(52.789038487168,-33.3645169267754,-45.));
#25445=CARTESIAN_POINT('',(52.789038487168,-33.3645169267754,-45.));
#25446=CARTESIAN_POINT('',(23.6909146109103,-57.7807419392945,-45.));
#25447=CARTESIAN_POINT('',(23.6909146109103,-57.7807419392945,-45.));
#25448=CARTESIAN_POINT('',(18.9924515069803,-59.4908426559229,-45.));
#25449=CARTESIAN_POINT('',(18.9924515069808,-59.4908426559229,-45.));
#25450=CARTESIAN_POINT('',(18.9924515069808,-59.4908426559229,-45.));
#25451=CARTESIAN_POINT('',(-18.99245150698,-59.4908426559232,-45.));
#25452=CARTESIAN_POINT('',(-18.99245150698,-59.4908426559232,-45.));
#25453=CARTESIAN_POINT('',(-23.6909146109095,-57.7807419392947,-45.));
#25454=CARTESIAN_POINT('',(-23.6909146109095,-57.7807419392948,-45.));
#25455=CARTESIAN_POINT('',(-23.6909146109095,-57.7807419392948,-45.));
#25456=CARTESIAN_POINT('',(-52.7890384871676,-33.3645169267762,-45.));
#25457=CARTESIAN_POINT('',(-52.7890384871676,-33.3645169267762,-45.));
#25458=CARTESIAN_POINT('',(-55.2890384871676,-29.0343899078537,-45.));
#25459=CARTESIAN_POINT('',(-55.2890384871676,-29.034389907854,-45.));
#25460=CARTESIAN_POINT('',(-55.2890384871676,-29.034389907854,-45.));
#25461=CARTESIAN_POINT('',(-61.8850476743971,8.3734370777113,-45.));
#25462=CARTESIAN_POINT('',(-61.8850476743971,8.3734370777113,-45.));
#25463=CARTESIAN_POINT('',(-61.0168067860623,13.2974758427723,-45.));
#25464=CARTESIAN_POINT('',(-61.0168067860625,13.2974758427723,-45.));
#25465=CARTESIAN_POINT('',(-61.0168067860625,13.2974758427723,-45.));
#25466=CARTESIAN_POINT('',(-42.0243552790822,46.1933668131505,-45.));
#25467=CARTESIAN_POINT('',(-42.0243552790822,46.1933668131505,-45.));
#25468=CARTESIAN_POINT('',(-38.194133063487,49.4073048615832,-45.));
#25469=CARTESIAN_POINT('',(-38.1941330634873,49.4073048615832,-45.));
#25470=CARTESIAN_POINT('',(-38.1941330634873,49.4073048615832,-45.));
#25471=CARTESIAN_POINT('',(-2.5,62.3989068346297,-45.));
#25472=CARTESIAN_POINT('',(-2.5,62.3989068346297,-45.));
#25473=CARTESIAN_POINT('',(2.5,62.3989068346295,-45.));
#25474=CARTESIAN_POINT('',(2.5,62.3989068346297,-45.));
#25475=CARTESIAN_POINT('',(2.5,62.3989068346297,-45.));
#25476=CARTESIAN_POINT('',(38.1941330634866,49.4073048615837,-45.));
#25477=CARTESIAN_POINT('',(38.1941330634866,49.4073048615837,-45.));
#25478=CARTESIAN_POINT('',(42.0243552790815,46.193366813151,-45.));
#25479=CARTESIAN_POINT('Origin',(0.,0.,55.));
#25480=CARTESIAN_POINT('Origin',(0.,0.,45.));
#25481=CARTESIAN_POINT('Origin',(0.,0.,-55.));
#25482=CARTESIAN_POINT('Origin',(263.115760998171,202.,-20.));
#25483=CARTESIAN_POINT('',(263.115760998171,197.,-20.));
#25484=CARTESIAN_POINT('',(263.115760998171,202.,-25.));
#25485=CARTESIAN_POINT('Origin',(263.115760998171,202.,-20.));
#25486=CARTESIAN_POINT('',(263.11576099817,242.,-25.));
#25487=CARTESIAN_POINT('',(263.115760998171,202.,-25.));
#25488=CARTESIAN_POINT('',(263.11576099817,247.,-20.));
#25489=CARTESIAN_POINT('Origin',(263.11576099817,242.,-20.));
#25490=CARTESIAN_POINT('',(263.11576099817,247.,20.));
#25491=CARTESIAN_POINT('',(263.11576099817,247.,20.));
#25492=CARTESIAN_POINT('',(263.11576099817,242.,25.));
#25493=CARTESIAN_POINT('Origin',(263.11576099817,242.,20.));
#25494=CARTESIAN_POINT('',(263.115760998171,202.,25.));
#25495=CARTESIAN_POINT('',(263.115760998171,202.,25.));
#25496=CARTESIAN_POINT('',(263.115760998171,197.,20.));
#25497=CARTESIAN_POINT('Origin',(263.115760998171,202.,20.));
#25498=CARTESIAN_POINT('',(263.115760998171,197.,20.));
#25499=CARTESIAN_POINT('Origin',(258.115760998171,202.,-20.));
#25500=CARTESIAN_POINT('',(258.115760998171,197.,-20.));
#25501=CARTESIAN_POINT('',(258.115760998171,202.,-25.));
#25502=CARTESIAN_POINT('Origin',(258.115760998171,202.,-20.));
#25503=CARTESIAN_POINT('',(258.115760998171,197.,20.));
#25504=CARTESIAN_POINT('',(258.115760998171,197.,20.));
#25505=CARTESIAN_POINT('',(258.115760998171,202.,25.));
#25506=CARTESIAN_POINT('Origin',(258.115760998171,202.,20.));
#25507=CARTESIAN_POINT('',(258.11576099817,242.,25.));
#25508=CARTESIAN_POINT('',(258.115760998171,202.,25.));
#25509=CARTESIAN_POINT('',(258.11576099817,247.,20.));
#25510=CARTESIAN_POINT('Origin',(258.11576099817,242.,20.));
#25511=CARTESIAN_POINT('',(258.11576099817,247.,-20.));
#25512=CARTESIAN_POINT('',(258.11576099817,247.,20.));
#25513=CARTESIAN_POINT('',(258.11576099817,242.,-25.));
#25514=CARTESIAN_POINT('Origin',(258.11576099817,242.,-20.));
#25515=CARTESIAN_POINT('',(258.115760998171,202.,-25.));
#25516=CARTESIAN_POINT('Origin',(263.115760998171,202.,-20.));
#25517=CARTESIAN_POINT('',(263.115760998171,202.,-25.));
#25518=CARTESIAN_POINT('',(263.115760998171,197.,-20.));
#25519=CARTESIAN_POINT('Origin',(263.115760998171,202.,-25.));
#25520=CARTESIAN_POINT('',(263.11576099817,242.,-25.));
#25521=CARTESIAN_POINT('Origin',(263.11576099817,242.,-20.));
#25522=CARTESIAN_POINT('',(263.11576099817,247.,-20.));
#25523=CARTESIAN_POINT('Origin',(263.11576099817,247.,20.));
#25524=CARTESIAN_POINT('',(263.11576099817,247.,20.));
#25525=CARTESIAN_POINT('Origin',(263.11576099817,242.,20.));
#25526=CARTESIAN_POINT('',(263.11576099817,242.,25.));
#25527=CARTESIAN_POINT('Origin',(263.115760998171,202.,25.));
#25528=CARTESIAN_POINT('',(263.115760998171,202.,25.));
#25529=CARTESIAN_POINT('Origin',(263.115760998171,202.,20.));
#25530=CARTESIAN_POINT('',(263.115760998171,197.,20.));
#25531=CARTESIAN_POINT('Origin',(263.115760998171,197.,20.));
#25532=CARTESIAN_POINT('Origin',(263.115760998171,-242.,-20.));
#25533=CARTESIAN_POINT('',(263.115760998171,-247.,-20.));
#25534=CARTESIAN_POINT('',(263.115760998171,-242.,-25.));
#25535=CARTESIAN_POINT('Origin',(263.115760998171,-242.,-20.));
#25536=CARTESIAN_POINT('',(263.115760998171,-202.,-25.));
#25537=CARTESIAN_POINT('',(263.115760998171,-202.,-25.));
#25538=CARTESIAN_POINT('',(263.115760998171,-197.,-20.));
#25539=CARTESIAN_POINT('Origin',(263.115760998171,-202.,-20.));
#25540=CARTESIAN_POINT('',(263.115760998171,-197.,20.));
#25541=CARTESIAN_POINT('',(263.115760998171,-197.,20.));
#25542=CARTESIAN_POINT('',(263.115760998171,-202.,25.));
#25543=CARTESIAN_POINT('Origin',(263.115760998171,-202.,20.));
#25544=CARTESIAN_POINT('',(263.115760998171,-242.,25.));
#25545=CARTESIAN_POINT('',(263.115760998171,-202.,25.));
#25546=CARTESIAN_POINT('',(263.115760998171,-247.,20.));
#25547=CARTESIAN_POINT('Origin',(263.115760998171,-242.,20.));
#25548=CARTESIAN_POINT('',(263.115760998171,-247.,20.));
#25549=CARTESIAN_POINT('Origin',(258.115760998171,-242.,-20.));
#25550=CARTESIAN_POINT('',(258.115760998171,-247.,-20.));
#25551=CARTESIAN_POINT('',(258.115760998171,-242.,-25.));
#25552=CARTESIAN_POINT('Origin',(258.115760998171,-242.,-20.));
#25553=CARTESIAN_POINT('',(258.115760998171,-247.,20.));
#25554=CARTESIAN_POINT('',(258.115760998171,-247.,20.));
#25555=CARTESIAN_POINT('',(258.115760998171,-242.,25.));
#25556=CARTESIAN_POINT('Origin',(258.115760998171,-242.,20.));
#25557=CARTESIAN_POINT('',(258.115760998171,-202.,25.));
#25558=CARTESIAN_POINT('',(258.115760998171,-202.,25.));
#25559=CARTESIAN_POINT('',(258.115760998171,-197.,20.));
#25560=CARTESIAN_POINT('Origin',(258.115760998171,-202.,20.));
#25561=CARTESIAN_POINT('',(258.115760998171,-197.,-20.));
#25562=CARTESIAN_POINT('',(258.115760998171,-197.,20.));
#25563=CARTESIAN_POINT('',(258.115760998171,-202.,-25.));
#25564=CARTESIAN_POINT('Origin',(258.115760998171,-202.,-20.));
#25565=CARTESIAN_POINT('',(258.115760998171,-202.,-25.));
#25566=CARTESIAN_POINT('Origin',(263.115760998171,-242.,-20.));
#25567=CARTESIAN_POINT('',(263.115760998171,-242.,-25.));
#25568=CARTESIAN_POINT('',(263.115760998171,-247.,-20.));
#25569=CARTESIAN_POINT('Origin',(263.115760998171,-202.,-25.));
#25570=CARTESIAN_POINT('',(263.115760998171,-202.,-25.));
#25571=CARTESIAN_POINT('Origin',(263.115760998171,-202.,-20.));
#25572=CARTESIAN_POINT('',(263.115760998171,-197.,-20.));
#25573=CARTESIAN_POINT('Origin',(263.115760998171,-197.,20.));
#25574=CARTESIAN_POINT('',(263.115760998171,-197.,20.));
#25575=CARTESIAN_POINT('Origin',(263.115760998171,-202.,20.));
#25576=CARTESIAN_POINT('',(263.115760998171,-202.,25.));
#25577=CARTESIAN_POINT('Origin',(263.115760998171,-202.,25.));
#25578=CARTESIAN_POINT('',(263.115760998171,-242.,25.));
#25579=CARTESIAN_POINT('Origin',(263.115760998171,-242.,20.));
#25580=CARTESIAN_POINT('',(263.115760998171,-247.,20.));
#25581=CARTESIAN_POINT('Origin',(263.115760998171,-247.,20.));
#25582=CARTESIAN_POINT('Origin',(0.,0.,-35.));
#25583=CARTESIAN_POINT('Origin',(2.5,0.,0.));
#25584=CARTESIAN_POINT('',(2.5,30.,-35.));
#25585=CARTESIAN_POINT('Origin',(-2.5,0.,0.));
#25586=CARTESIAN_POINT('',(-2.5,30.,-35.));
#25587=CARTESIAN_POINT('Origin',(2.5,30.,-35.));
#25588=CARTESIAN_POINT('Origin',(1.91511110779744,1.60696902421635,0.));
#25589=CARTESIAN_POINT('',(-17.3685171827988,24.5883023177857,-35.));
#25590=CARTESIAN_POINT('Origin',(-1.91511110779744,-1.60696902421635,0.));
#25591=CARTESIAN_POINT('',(-21.1987393983937,21.374364269353,-35.));
#25592=CARTESIAN_POINT('Origin',(-17.3685171827988,24.5883023177857,-35.));
#25593=CARTESIAN_POINT('Origin',(0.434120444167318,2.46201938253052,0.));
#25594=CARTESIAN_POINT('',(-29.1101121461989,7.67146471253834,-35.));
#25595=CARTESIAN_POINT('Origin',(-0.434120444167318,-2.46201938253052,0.));
#25596=CARTESIAN_POINT('',(-29.9783530345336,2.7474259474773,-35.));
#25597=CARTESIAN_POINT('Origin',(-29.1101121461989,7.67146471253834,-35.));
#25598=CARTESIAN_POINT('Origin',(-1.25000000000001,2.16506350946109,0.));
#25599=CARTESIAN_POINT('',(-27.2307621135331,-12.834936490539,-35.));
#25600=CARTESIAN_POINT('Origin',(1.25000000000001,-2.16506350946109,0.));
#25601=CARTESIAN_POINT('',(-24.7307621135331,-17.1650635094612,-35.));
#25602=CARTESIAN_POINT('Origin',(-27.2307621135331,-12.834936490539,-35.));
#25603=CARTESIAN_POINT('Origin',(-2.34923155196478,0.855050358314158,0.));
#25604=CARTESIAN_POINT('',(-12.6098358517347,-27.3357282652632,-35.));
#25605=CARTESIAN_POINT('Origin',(2.34923155196478,-0.855050358314158,0.));
#25606=CARTESIAN_POINT('',(-7.91137274780512,-29.0458289818915,-35.));
#25607=CARTESIAN_POINT('Origin',(-12.6098358517347,-27.3357282652632,-35.));
#25608=CARTESIAN_POINT('Origin',(-2.34923155196477,-0.855050358314189,0.));
#25609=CARTESIAN_POINT('',(7.91137274780551,-29.0458289818914,-35.));
#25610=CARTESIAN_POINT('Origin',(2.34923155196477,0.855050358314189,0.));
#25611=CARTESIAN_POINT('',(12.609835851735,-27.335728265263,-35.));
#25612=CARTESIAN_POINT('Origin',(7.91137274780551,-29.0458289818914,-35.));
#25613=CARTESIAN_POINT('Origin',(-1.24999999999998,-2.16506350946111,0.));
#25614=CARTESIAN_POINT('',(24.7307621135333,-17.1650635094609,-35.));
#25615=CARTESIAN_POINT('Origin',(1.24999999999998,2.16506350946111,0.));
#25616=CARTESIAN_POINT('',(27.2307621135333,-12.8349364905386,-35.));
#25617=CARTESIAN_POINT('Origin',(24.7307621135333,-17.1650635094609,-35.));
#25618=CARTESIAN_POINT('Origin',(0.434120444167351,-2.46201938253052,0.));
#25619=CARTESIAN_POINT('',(29.9783530345335,2.7474259474777,-35.));
#25620=CARTESIAN_POINT('Origin',(-0.434120444167351,2.46201938253052,0.));
#25621=CARTESIAN_POINT('',(29.1101121461988,7.67146471253873,-35.));
#25622=CARTESIAN_POINT('Origin',(29.9783530345335,2.7474259474777,-35.));
#25623=CARTESIAN_POINT('Origin',(1.91511110779746,-1.60696902421633,0.));
#25624=CARTESIAN_POINT('',(21.1987393983934,21.3743642693533,-35.));
#25625=CARTESIAN_POINT('Origin',(-1.91511110779746,1.60696902421633,0.));
#25626=CARTESIAN_POINT('',(17.3685171827984,24.5883023177859,-35.));
#25627=CARTESIAN_POINT('Origin',(21.1987393983934,21.3743642693533,-35.));
#25628=CARTESIAN_POINT('',(0.,0.,0.));
#25629=CARTESIAN_POINT('Origin',(6.93889390390723E-15,1.21430643318376E-14,
-7.));
#25630=CARTESIAN_POINT('',(-184.50486486776,-91.6185289127127,-7.));
#25631=CARTESIAN_POINT('',(-184.50486486776,91.6185289127127,-7.));
#25632=CARTESIAN_POINT('Origin',(6.93889390390723E-15,1.21430643318376E-14,
-7.));
#25633=CARTESIAN_POINT('',(-184.50486486776,91.6185289127127,-10.));
#25634=CARTESIAN_POINT('',(-184.50486486776,91.6185289127127,-7.));
#25635=CARTESIAN_POINT('',(-184.50486486776,-91.6185289127127,-10.));
#25636=CARTESIAN_POINT('Origin',(6.93889390390723E-15,1.21430643318376E-14,
-10.));
#25637=CARTESIAN_POINT('',(-184.50486486776,-91.6185289127127,-7.));
#25638=CARTESIAN_POINT('Origin',(-71.5953323638214,6.93889390390723E-15,
-7.));
#25639=CARTESIAN_POINT('Origin',(-71.5953323638214,6.93889390390723E-15,
-7.));
#25640=CARTESIAN_POINT('Origin',(-71.5953323638214,6.93889390390723E-15,
-10.));
#25641=CARTESIAN_POINT('Origin',(-210.,0.,0.));
#25642=CARTESIAN_POINT('',(-210.,-6.12323399573677E-16,5.));
#25643=CARTESIAN_POINT('Origin',(-210.,0.,0.));
#25644=CARTESIAN_POINT('',(-204.,-1.32734112397626E-14,5.));
#25645=CARTESIAN_POINT('',(-210.,-6.12323399573677E-16,5.));
#25646=CARTESIAN_POINT('',(-203.969359287593,-3.53561414983974,3.53545365999116));
#25647=CARTESIAN_POINT('Ctrl Pts',(-203.969360444161,-3.53553390593274,
3.53553390593274));
#25648=CARTESIAN_POINT('Ctrl Pts',(-203.977055116563,-3.09161865850825,
3.97944915335723));
#25649=CARTESIAN_POINT('Ctrl Pts',(-203.985248421744,-2.52939665845125,
4.36424514979789));
#25650=CARTESIAN_POINT('Ctrl Pts',(-203.996803640531,-1.29750744995471,
4.8745212692142));
#25651=CARTESIAN_POINT('Ctrl Pts',(-204.,-0.627838117491496,5.));
#25652=CARTESIAN_POINT('Ctrl Pts',(-204.,-6.93889390390723E-16,5.));
#25653=CARTESIAN_POINT('',(-203.938716194739,-4.99999958112187,0.00204287664667749));
#25654=CARTESIAN_POINT('Ctrl Pts',(-203.938716295296,-4.99999958266548,
0.00204287664629751));
#25655=CARTESIAN_POINT('Ctrl Pts',(-203.938722578506,-4.99974330468984,
0.629290622414902));
#25656=CARTESIAN_POINT('Ctrl Pts',(-203.941919986053,-4.87424456118115,
1.29817546531228));
#25657=CARTESIAN_POINT('Ctrl Pts',(-203.953470693038,-4.36427603534107,
2.52932209840595));
#25658=CARTESIAN_POINT('Ctrl Pts',(-203.961663784593,-3.97954354876496,
3.09148377916774));
#25659=CARTESIAN_POINT('Ctrl Pts',(-203.969357649916,-3.53569510571298,
3.53537269880239));
#25660=CARTESIAN_POINT('',(-203.969331848638,-3.53718156034075,-3.53388548308072));
#25661=CARTESIAN_POINT('Ctrl Pts',(-203.96933187763,-3.5371815607091,-3.53388548294644));
#25662=CARTESIAN_POINT('Ctrl Pts',(-203.961645461725,-3.98041386013988,
-3.09023977789374));
#25663=CARTESIAN_POINT('Ctrl Pts',(-203.953464241805,-4.36456085996178,
-2.52863448563173));
#25664=CARTESIAN_POINT('Ctrl Pts',(-203.941913718727,-4.87452126623505,
-1.29750745448768));
#25665=CARTESIAN_POINT('Ctrl Pts',(-203.938716285064,-5.,-0.627838125135884));
#25666=CARTESIAN_POINT('Ctrl Pts',(-203.938716285064,-5.,0.));
#25667=CARTESIAN_POINT('Ctrl Pts',(-203.938716285064,-5.,0.000680909716903597));
#25668=CARTESIAN_POINT('Ctrl Pts',(-203.938716288475,-4.99999986090858,
0.00136186863985322));
#25669=CARTESIAN_POINT('Ctrl Pts',(-203.938716295296,-4.99999958266548,
0.00204287664629765));
#25670=CARTESIAN_POINT('',(-203.99999999855,-0.000260375111436809,-4.99999993829161));
#25671=CARTESIAN_POINT('Ctrl Pts',(-203.999999999834,-0.000260375114298633,
-4.99999999322048));
#25672=CARTESIAN_POINT('Ctrl Pts',(-203.99999919859,-0.628023263685998,
-4.99996730245366));
#25673=CARTESIAN_POINT('Ctrl Pts',(-203.996802841847,-1.29759259672811,
-4.87448599951234));
#25674=CARTESIAN_POINT('Ctrl Pts',(-203.985248421744,-2.52939665845125,
-4.36424514979789));
#25675=CARTESIAN_POINT('Ctrl Pts',(-203.977055116563,-3.09161865850825,
-3.97944915335723));
#25676=CARTESIAN_POINT('Ctrl Pts',(-203.969350922768,-3.53608320695274,
-3.53498460491273));
#25677=CARTESIAN_POINT('Ctrl Pts',(-203.969341400589,-3.53663242527553,
-3.53443513056216));
#25678=CARTESIAN_POINT('Ctrl Pts',(-203.96933187763,-3.5371815607091,-3.53388548294644));
#25679=CARTESIAN_POINT('',(-203.969412573458,3.53252077317422,-3.53854447085706));
#25680=CARTESIAN_POINT('Ctrl Pts',(-203.969412650463,3.53252077489201,-3.53854447124186));
#25681=CARTESIAN_POINT('Ctrl Pts',(-203.977092222053,3.0890986957704,-3.98121170893611));
#25682=CARTESIAN_POINT('Ctrl Pts',(-203.985261486298,2.52800386071199,-4.36482207783705));
#25683=CARTESIAN_POINT('Ctrl Pts',(-203.996803640531,1.29750744995471,-4.8745212692142));
#25684=CARTESIAN_POINT('Ctrl Pts',(-204.,0.627838117491497,-5.));
#25685=CARTESIAN_POINT('Ctrl Pts',(-204.,1.11022302462516E-15,-5.));
#25686=CARTESIAN_POINT('',(-203.938716348762,4.99999732701828,-0.00517006110607621));
#25687=CARTESIAN_POINT('Ctrl Pts',(-203.938716350598,4.9999973270461,-0.0051700611060565));
#25688=CARTESIAN_POINT('Ctrl Pts',(-203.938732229062,4.99934967998715,-0.631513444132154));
#25689=CARTESIAN_POINT('Ctrl Pts',(-203.94192957817,4.87382106523366,-1.29919785313323));
#25690=CARTESIAN_POINT('Ctrl Pts',(-203.953471392542,4.36424515196542,-2.52939665587767));
#25691=CARTESIAN_POINT('Ctrl Pts',(-203.961665771665,3.97944915876222,-3.09161865310325));
#25692=CARTESIAN_POINT('Ctrl Pts',(-203.969377843651,3.53453010762235,-3.53653770424313));
#25693=CARTESIAN_POINT('Ctrl Pts',(-203.969395245763,3.53352573047557,-3.53754122640331));
#25694=CARTESIAN_POINT('Ctrl Pts',(-203.969412650463,3.53252077489201,-3.53854447124186));
#25695=CARTESIAN_POINT('',(-203.969318710503,3.53793517768081,3.53313100014201));
#25696=CARTESIAN_POINT('Ctrl Pts',(-203.969318807181,3.53793517953451,3.53313100031857));
#25697=CARTESIAN_POINT('Ctrl Pts',(-203.961636172418,3.98085504657878,3.08960887244123));
#25698=CARTESIAN_POINT('Ctrl Pts',(-203.953460970419,4.3647052930154,2.52828580084305));
#25699=CARTESIAN_POINT('Ctrl Pts',(-203.941913718727,4.87452126623505,1.29750745448768));
#25700=CARTESIAN_POINT('Ctrl Pts',(-203.938716285064,5.,0.627838125135884));
#25701=CARTESIAN_POINT('Ctrl Pts',(-203.938716285064,5.,-0.00172303923949561));
#25702=CARTESIAN_POINT('Ctrl Pts',(-203.938716306901,4.99999910934032,-0.00344639360360825));
#25703=CARTESIAN_POINT('Ctrl Pts',(-203.938716350598,4.9999973270461,-0.0051700611060567));
#25704=CARTESIAN_POINT('Ctrl Pts',(-204.,-4.16333634234434E-16,5.));
#25705=CARTESIAN_POINT('Ctrl Pts',(-204.,0.627838117491495,5.));
#25706=CARTESIAN_POINT('Ctrl Pts',(-203.996803640531,1.29750744995471,4.8745212692142));
#25707=CARTESIAN_POINT('Ctrl Pts',(-203.985248421744,2.52939665845125,4.36424514979789));
#25708=CARTESIAN_POINT('Ctrl Pts',(-203.977055116563,3.09161865850825,3.97944915335723));
#25709=CARTESIAN_POINT('Ctrl Pts',(-203.969346566832,3.53633450633251,3.53473330553297));
#25710=CARTESIAN_POINT('Ctrl Pts',(-203.969332687833,3.53713493106456,3.53393233692737));
#25711=CARTESIAN_POINT('Ctrl Pts',(-203.969318807181,3.53793517953451,3.53313100031857));
#25712=CARTESIAN_POINT('Origin',(-71.5953323638214,6.93889390390723E-15,
10.));
#25713=CARTESIAN_POINT('',(-174.6884520924,105.356275112407,10.));
#25714=CARTESIAN_POINT('',(-174.6884520924,-105.356275112407,10.));
#25715=CARTESIAN_POINT('Origin',(-71.5953323638214,6.93889390390723E-15,
10.));
#25716=CARTESIAN_POINT('',(-174.6884520924,105.356275112407,-10.));
#25717=CARTESIAN_POINT('',(-174.6884520924,105.356275112407,10.));
#25718=CARTESIAN_POINT('',(-174.6884520924,-105.356275112407,-10.));
#25719=CARTESIAN_POINT('Origin',(-71.5953323638214,6.93889390390723E-15,
-10.));
#25720=CARTESIAN_POINT('',(-174.6884520924,-105.356275112407,10.));
#25721=CARTESIAN_POINT('Origin',(-35.7976661819107,9.54097911787244E-15,
-10.));
#25722=CARTESIAN_POINT('Origin',(6.93889390390723E-15,1.21430643318376E-14,
-10.));
#25723=CARTESIAN_POINT('Origin',(-35.7976661819107,9.54097911787244E-15,
10.));
#25724=CARTESIAN_POINT('Origin',(6.93889390390723E-15,1.21430643318376E-14,
10.));
#25725=CARTESIAN_POINT('',(-184.50486486776,91.6185289127127,10.));
#25726=CARTESIAN_POINT('',(-184.50486486776,-91.6185289127127,10.));
#25727=CARTESIAN_POINT('Origin',(-71.5953323638214,6.93889390390723E-15,
10.));
#25728=CARTESIAN_POINT('Origin',(6.93889390390723E-15,1.21430643318376E-14,
10.));
#25729=CARTESIAN_POINT('Origin',(-210.,0.,0.));
#25730=CARTESIAN_POINT('Origin',(-71.5953323638214,6.93889390390723E-15,
7.));
#25731=CARTESIAN_POINT('',(-184.50486486776,-91.6185289127127,7.));
#25732=CARTESIAN_POINT('',(-184.50486486776,-91.6185289127127,7.));
#25733=CARTESIAN_POINT('',(-184.50486486776,91.6185289127127,7.));
#25734=CARTESIAN_POINT('Origin',(-71.5953323638214,6.93889390390723E-15,
7.));
#25735=CARTESIAN_POINT('',(-184.50486486776,91.6185289127127,7.));
#25736=CARTESIAN_POINT('Origin',(6.93889390390723E-15,1.21430643318376E-14,
7.));
#25737=CARTESIAN_POINT('Origin',(6.93889390390723E-15,1.21430643318376E-14,
7.));
#25738=CARTESIAN_POINT('Origin',(-35.7976661819107,9.54097911787244E-15,
7.));
#25739=CARTESIAN_POINT('Origin',(-35.7976661819107,9.54097911787244E-15,
-7.));
#25740=CARTESIAN_POINT('Origin',(6.93889390390723E-15,1.21430643318376E-14,
12.5));
#25741=CARTESIAN_POINT('Ctrl Pts',(-203.969357610281,-3.53569510523211,
3.53537269900855));
#25742=CARTESIAN_POINT('Ctrl Pts',(-203.969356693716,-3.53574798064454,
3.53531981895734));
#25743=CARTESIAN_POINT('Ctrl Pts',(-203.969355777146,-3.53580085486419,
3.53526693763481));
#25744=CARTESIAN_POINT('Ctrl Pts',(-203.969354860571,-3.53585372789099,
3.53521405504099));
#25745=CARTESIAN_POINT('Ctrl Pts',(-203.969353523271,-3.5359308706626,3.53513689831092));
#25746=CARTESIAN_POINT('Ctrl Pts',(-203.969352185979,-3.53600801081182,
3.5350597388574));
#25747=CARTESIAN_POINT('Ctrl Pts',(-203.969350848697,-3.53608514833853,
3.53498257668063));
#25748=CARTESIAN_POINT('Ctrl Pts',(-203.968102971582,-3.60806555270628,
3.46297917027145));
#25749=CARTESIAN_POINT('Ctrl Pts',(-203.966863395218,-3.67743065556072,
3.38894263048284));
#25750=CARTESIAN_POINT('Ctrl Pts',(-203.965637313051,-3.74428389561946,
3.31295292278655));
#25751=CARTESIAN_POINT('Ctrl Pts',(-203.964393266827,-3.81211664212436,
3.23584984484127));
#25752=CARTESIAN_POINT('Ctrl Pts',(-203.963163096211,-3.877363644099,3.15673552555768));
#25753=CARTESIAN_POINT('Ctrl Pts',(-203.961952291397,-3.94009625713642,
3.07565384174656));
#25754=CARTESIAN_POINT('Ctrl Pts',(-203.960730121248,-4.00341771586461,
2.99381107693147));
#25755=CARTESIAN_POINT('Ctrl Pts',(-203.959527664023,-4.06417763323105,
2.90996337813423));
#25756=CARTESIAN_POINT('Ctrl Pts',(-203.958350897716,-4.122408262698,2.82412250980142));
#25757=CARTESIAN_POINT('Ctrl Pts',(-203.957172007328,-4.18074399933042,
2.73812669740508));
#25758=CARTESIAN_POINT('Ctrl Pts',(-203.956018882071,-4.23654156600736,
2.65013001319041));
#25759=CARTESIAN_POINT('Ctrl Pts',(-203.954898139835,-4.28978839858892,
2.56011827232567));
#25760=CARTESIAN_POINT('Ctrl Pts',(-203.953783867703,-4.34272783439241,
2.47062617399722));
#25761=CARTESIAN_POINT('Ctrl Pts',(-203.952701587561,-4.39314613126717,
2.37914170259479));
#25762=CARTESIAN_POINT('Ctrl Pts',(-203.951658676823,-4.44098296523244,
2.28563285085449));
#25763=CARTESIAN_POINT('Ctrl Pts',(-203.950633072017,-4.48802600064509,
2.19367567352523));
#25764=CARTESIAN_POINT('Ctrl Pts',(-203.949645524783,-4.53257269388454,
2.09976023710277));
#25765=CARTESIAN_POINT('Ctrl Pts',(-203.948704148847,-4.57451641576525,
2.00384615015072));
#25766=CARTESIAN_POINT('Ctrl Pts',(-203.948404891615,-4.58785004969342,
1.97335569134953));
#25767=CARTESIAN_POINT('Ctrl Pts',(-203.948110309694,-4.60092024898877,
1.94266321081319));
#25768=CARTESIAN_POINT('Ctrl Pts',(-203.947820691679,-4.61372247670505,
1.91176732253888));
#25769=CARTESIAN_POINT('Ctrl Pts',(-203.946912093852,-4.65388598749793,
1.81483986821907));
#25770=CARTESIAN_POINT('Ctrl Pts',(-203.946063611632,-4.6907675717227,1.7174757848906));
#25771=CARTESIAN_POINT('Ctrl Pts',(-203.945278888644,-4.7244863460725,1.61972835506864));
#25772=CARTESIAN_POINT('Ctrl Pts',(-203.944484940015,-4.75860153715152,
1.5208317519103));
#25773=CARTESIAN_POINT('Ctrl Pts',(-203.943756240949,-4.78947932184167,
1.42154221971967));
#25774=CARTESIAN_POINT('Ctrl Pts',(-203.94309699481,-4.81719984076717,1.32188335555093));
#25775=CARTESIAN_POINT('Ctrl Pts',(-203.942432162295,-4.84515526023121,
1.22137999345174));
#25776=CARTESIAN_POINT('Ctrl Pts',(-203.941837946665,-4.8698998937537,1.12050048682021));
#25777=CARTESIAN_POINT('Ctrl Pts',(-203.941319364095,-4.89146906173073,
1.01924502824124));
#25778=CARTESIAN_POINT('Ctrl Pts',(-203.941232999844,-4.89506117054544,
1.00238204003108));
#25779=CARTESIAN_POINT('Ctrl Pts',(-203.941148735228,-4.89856509815127,
0.985508581542827));
#25780=CARTESIAN_POINT('Ctrl Pts',(-203.941066595844,-4.90198087606653,
0.968624605516958));
#25781=CARTESIAN_POINT('Ctrl Pts',(-203.94063972183,-4.91973249253479,0.880879478548298));
#25782=CARTESIAN_POINT('Ctrl Pts',(-203.94027118057,-4.9350824150589,0.79297491825541));
#25783=CARTESIAN_POINT('Ctrl Pts',(-203.939960217077,-4.94804802325662,
0.704798382938753));
#25784=CARTESIAN_POINT('Ctrl Pts',(-203.939651507015,-4.9609196747494,0.617260828577294));
#25785=CARTESIAN_POINT('Ctrl Pts',(-203.939399529957,-4.97144155245078,
0.52945478342709));
#25786=CARTESIAN_POINT('Ctrl Pts',(-203.939204733522,-4.97958027609786,
0.44126268565492));
#25787=CARTESIAN_POINT('Ctrl Pts',(-203.9390135821,-4.9875667087051,0.354720830212983));
#25788=CARTESIAN_POINT('Ctrl Pts',(-203.938877480764,-4.99325838390049,
0.267806829941029));
#25789=CARTESIAN_POINT('Ctrl Pts',(-203.938798171246,-4.99657408274633,
0.180408643921277));
#25790=CARTESIAN_POINT('Ctrl Pts',(-203.938744615543,-4.99881308995086,
0.12139086900888));
#25791=CARTESIAN_POINT('Ctrl Pts',(-203.938716983673,-4.99996764782323,
0.062152291453425));
#25792=CARTESIAN_POINT('Ctrl Pts',(-203.938716201879,-4.99999929267631,
0.00265955567477993));
#25793=CARTESIAN_POINT('Ctrl Pts',(-203.938716200513,-4.99999934795696,
0.00255562733875602));
#25794=CARTESIAN_POINT('Ctrl Pts',(-203.938716199228,-4.99999939986611,
0.00245169825933746));
#25795=CARTESIAN_POINT('Ctrl Pts',(-203.938716198025,-4.99999944840367,
0.00234776843634019));
#25796=CARTESIAN_POINT('Ctrl Pts',(-203.938716196848,-4.99999949586766,
0.00224613737482393));
#25797=CARTESIAN_POINT('Ctrl Pts',(-203.938716195753,-4.99999954010701,
0.00214450677827265));
#25798=CARTESIAN_POINT('Ctrl Pts',(-203.938716194739,-4.99999958112187,
0.00204287664667743));
#25799=CARTESIAN_POINT('Origin',(6.93889390390723E-15,1.21430643318376E-14,
12.5));
#25800=CARTESIAN_POINT('Ctrl Pts',(-204.,-1.32734112397625E-14,5.));
#25801=CARTESIAN_POINT('Ctrl Pts',(-204.,-0.105934998674852,5.));
#25802=CARTESIAN_POINT('Ctrl Pts',(-203.999905939126,-0.211337971606702,
4.99651966715266));
#25803=CARTESIAN_POINT('Ctrl Pts',(-203.999725729962,-0.316230501501799,
4.98968355835091));
#25804=CARTESIAN_POINT('Ctrl Pts',(-203.999538700243,-0.425093003726101,
4.98258871651251));
#25805=CARTESIAN_POINT('Ctrl Pts',(-203.999258867793,-0.533406187565095,
4.9718793685295));
#25806=CARTESIAN_POINT('Ctrl Pts',(-203.998893507736,-0.64119150817493,
4.95763708121322));
#25807=CARTESIAN_POINT('Ctrl Pts',(-203.998532826796,-0.74759643673455,
4.94357719294793));
#25808=CARTESIAN_POINT('Ctrl Pts',(-203.998088773486,-0.853487399797586,
4.92607394237269));
#25809=CARTESIAN_POINT('Ctrl Pts',(-203.997567101389,-0.958875298258525,
4.90515317922688));
#25810=CARTESIAN_POINT('Ctrl Pts',(-203.997045990193,-1.0641498837675,4.8842549100625));
#25811=CARTESIAN_POINT('Ctrl Pts',(-203.996447409029,-1.16892297110147,
4.85994627755904));
#25812=CARTESIAN_POINT('Ctrl Pts',(-203.995776131441,-1.27318855674928,
4.8322039916926));
#25813=CARTESIAN_POINT('Ctrl Pts',(-203.995109685905,-1.37670360839317,
4.80466140286675));
#25814=CARTESIAN_POINT('Ctrl Pts',(-203.994371568543,-1.47971891143702,
4.77373420137415));
#25815=CARTESIAN_POINT('Ctrl Pts',(-203.993565773266,-1.58220484941587,
4.73935434229579));
#25816=CARTESIAN_POINT('Ctrl Pts',(-203.992732918314,-1.68813240120964,
4.70381996192122));
#25817=CARTESIAN_POINT('Ctrl Pts',(-203.991827746257,-1.79349523021465,
4.66459724220142));
#25818=CARTESIAN_POINT('Ctrl Pts',(-203.990854206795,-1.89822529428719,
4.62156297086283));
#25819=CARTESIAN_POINT('Ctrl Pts',(-203.990755308256,-1.90886446274436,
4.61719126665108));
#25820=CARTESIAN_POINT('Ctrl Pts',(-203.990655669341,-1.91950065693411,
4.61277864479938));
#25821=CARTESIAN_POINT('Ctrl Pts',(-203.990555535075,-1.93010846927917,
4.60833566613732));
#25822=CARTESIAN_POINT('Ctrl Pts',(-203.989623947544,-2.02879702187669,
4.56700092914183));
#25823=CARTESIAN_POINT('Ctrl Pts',(-203.988645783478,-2.12544454260582,
4.52287513049451));
#25824=CARTESIAN_POINT('Ctrl Pts',(-203.987628217859,-2.22009981897521,
4.47607498314025));
#25825=CARTESIAN_POINT('Ctrl Pts',(-203.986576674134,-2.31791578307618,
4.4277121056641));
#25826=CARTESIAN_POINT('Ctrl Pts',(-203.985483038528,-2.41360478322964,
4.3764932632756));
#25827=CARTESIAN_POINT('Ctrl Pts',(-203.984353960946,-2.50720785336269,
4.32249107453453));
#25828=CARTESIAN_POINT('Ctrl Pts',(-203.983224883364,-2.60081092349573,
4.26848888579346));
#25829=CARTESIAN_POINT('Ctrl Pts',(-203.982060342399,-2.69232855862323,
4.21170304388256));
#25830=CARTESIAN_POINT('Ctrl Pts',(-203.980866027979,-2.78178136197962,
4.15215395164811));
#25831=CARTESIAN_POINT('Ctrl Pts',(-203.977955208569,-2.99979845363451,
4.00701909379552));
#25832=CARTESIAN_POINT('Ctrl Pts',(-203.974852066525,-3.20665944575788,
3.84469935011728));
#25833=CARTESIAN_POINT('Ctrl Pts',(-203.97166383987,-3.39947681026973,3.66637359289185));
#25834=CARTESIAN_POINT('Ctrl Pts',(-203.970899480465,-3.44570368867466,
3.62362099580809));
#25835=CARTESIAN_POINT('Ctrl Pts',(-203.970130239275,-3.49112317575354,
3.5799485388053));
#25836=CARTESIAN_POINT('Ctrl Pts',(-203.969357610281,-3.53569510523211,
3.53537269900855));
#25837=CARTESIAN_POINT('Origin',(6.93889390390723E-15,1.21430643318376E-14,
12.5));
#25838=CARTESIAN_POINT('Ctrl Pts',(-203.969318710503,3.53793517768081,3.53313100014201));
#25839=CARTESIAN_POINT('Ctrl Pts',(-203.969319343331,3.53789869384933,3.53316753322899));
#25840=CARTESIAN_POINT('Ctrl Pts',(-203.969319976156,3.53786220936332,3.53320406579359));
#25841=CARTESIAN_POINT('Ctrl Pts',(-203.969320608979,3.53782572422278,3.53324059783579));
#25842=CARTESIAN_POINT('Ctrl Pts',(-203.970611807987,3.46338221651318,3.60777980269651));
#25843=CARTESIAN_POINT('Ctrl Pts',(-203.971888843469,3.38684047652641,3.67952299153842));
#25844=CARTESIAN_POINT('Ctrl Pts',(-203.973147340404,3.30828782941231,3.7485675397376));
#25845=CARTESIAN_POINT('Ctrl Pts',(-203.974474867646,3.22542646040027,3.8213992773911));
#25846=CARTESIAN_POINT('Ctrl Pts',(-203.975781787315,3.14032736598223,3.89122878189774));
#25847=CARTESIAN_POINT('Ctrl Pts',(-203.977062936614,3.05304750252111,3.95812848589098));
#25848=CARTESIAN_POINT('Ctrl Pts',(-203.978344085913,2.96576763905998,4.02502818988422));
#25849=CARTESIAN_POINT('Ctrl Pts',(-203.979599486566,2.87630643596515,4.08899834926344));
#25850=CARTESIAN_POINT('Ctrl Pts',(-203.980823625848,2.78468276933246,4.15006483737447));
#25851=CARTESIAN_POINT('Ctrl Pts',(-203.981870899358,2.70629704939164,4.20230833308643));
#25852=CARTESIAN_POINT('Ctrl Pts',(-203.982894364117,2.62639950599981,4.2523802263174));
#25853=CARTESIAN_POINT('Ctrl Pts',(-203.983891257211,2.54490943418125,4.30032213736983));
#25854=CARTESIAN_POINT('Ctrl Pts',(-203.984884418463,2.46372441826546,4.3480845791614));
#25855=CARTESIAN_POINT('Ctrl Pts',(-203.985851223315,2.38095835588121,4.39373317038848));
#25856=CARTESIAN_POINT('Ctrl Pts',(-203.986788196368,2.29650898991706,4.43726262079967));
#25857=CARTESIAN_POINT('Ctrl Pts',(-203.987715596661,2.21292241663634,4.48034734446959));
#25858=CARTESIAN_POINT('Ctrl Pts',(-203.98861378765,2.12768634428916,4.52135620175186));
#25859=CARTESIAN_POINT('Ctrl Pts',(-203.989478428242,2.04068579461556,4.56023551915283));
#25860=CARTESIAN_POINT('Ctrl Pts',(-203.989733389213,2.01503149991839,4.57170006127321));
#25861=CARTESIAN_POINT('Ctrl Pts',(-203.989985425568,1.98922369851592,4.58297910210696));
#25862=CARTESIAN_POINT('Ctrl Pts',(-203.990234406414,1.96325925710145,4.59407040651396));
#25863=CARTESIAN_POINT('Ctrl Pts',(-203.990344101315,1.95181995613283,4.59895696529723));
#25864=CARTESIAN_POINT('Ctrl Pts',(-203.990453202995,1.9403502493567,4.60380707787955));
#25865=CARTESIAN_POINT('Ctrl Pts',(-203.990561699649,1.92884986487884,4.6086205279904));
#25866=CARTESIAN_POINT('Ctrl Pts',(-203.99064911369,1.91958418678222,4.61249864870428));
#25867=CARTESIAN_POINT('Ctrl Pts',(-203.990736158426,1.91029601075009,4.61635400051938));
#25868=CARTESIAN_POINT('Ctrl Pts',(-203.99082262093,1.90100758274172,4.62017734818583));
#25869=CARTESIAN_POINT('Ctrl Pts',(-203.9917505584,1.80132182385841,4.66121048245372));
#25870=CARTESIAN_POINT('Ctrl Pts',(-203.992616459951,1.70108357376192,4.69878322677367));
#25871=CARTESIAN_POINT('Ctrl Pts',(-203.993417023432,1.60035035707351,4.73300773477725));
#25872=CARTESIAN_POINT('Ctrl Pts',(-203.994226939003,1.49844038654684,4.76763204954248));
#25873=CARTESIAN_POINT('Ctrl Pts',(-203.994969999376,1.39602334141336,4.79882966441702));
#25874=CARTESIAN_POINT('Ctrl Pts',(-203.99564238175,1.29312684702631,4.8266737670285));
#25875=CARTESIAN_POINT('Ctrl Pts',(-203.996333096745,1.18742486192691,4.8552770439125));
#25876=CARTESIAN_POINT('Ctrl Pts',(-203.996949249375,1.08121648770143,4.88034184081964));
#25877=CARTESIAN_POINT('Ctrl Pts',(-203.997485958936,0.974505079806989,
4.90189757804557));
#25878=CARTESIAN_POINT('Ctrl Pts',(-203.998010132875,0.870286070072518,
4.92294985007637));
#25879=CARTESIAN_POINT('Ctrl Pts',(-203.998458545774,0.765586677755228,
4.94065505980157));
#25880=CARTESIAN_POINT('Ctrl Pts',(-203.998825695445,0.660392869034546,
4.95499142144511));
#25881=CARTESIAN_POINT('Ctrl Pts',(-203.999206015696,0.551425494589673,
4.96984206433358));
#25882=CARTESIAN_POINT('Ctrl Pts',(-203.999499166199,0.441927125126886,
4.98107840366953));
#25883=CARTESIAN_POINT('Ctrl Pts',(-203.999697656623,0.331871235928197,
4.98861781341002));
#25884=CARTESIAN_POINT('Ctrl Pts',(-203.999884886851,0.228058725888239,
4.99572951869974));
#25885=CARTESIAN_POINT('Ctrl Pts',(-203.999987896713,0.123749676165767,
4.99955156729294));
#25886=CARTESIAN_POINT('Ctrl Pts',(-203.999998997644,0.0189194210330657,
4.99996287881259));
#25887=CARTESIAN_POINT('Ctrl Pts',(-203.999999665264,0.0126148337550222,
4.99998761546301));
#25888=CARTESIAN_POINT('Ctrl Pts',(-204.,0.00630836177732318,5.));
#25889=CARTESIAN_POINT('Ctrl Pts',(-204.,1.11022302462516E-14,5.));
#25890=CARTESIAN_POINT('Origin',(6.93889390390723E-15,1.21430643318376E-14,
12.5));
#25891=CARTESIAN_POINT('Ctrl Pts',(-203.938716348762,4.99999732701828,-0.00517006110607632));
#25892=CARTESIAN_POINT('Ctrl Pts',(-203.93871634805,4.99999735605216,-0.00514200020558854));
#25893=CARTESIAN_POINT('Ctrl Pts',(-203.938716347344,4.99999738484058,-0.00511393926482346));
#25894=CARTESIAN_POINT('Ctrl Pts',(-203.938716346644,4.99999741338354,-0.00508587828380103));
#25895=CARTESIAN_POINT('Ctrl Pts',(-203.938716346556,4.9999974169859,-0.00508233675359046));
#25896=CARTESIAN_POINT('Ctrl Pts',(-203.938716346468,4.99999742058435,-0.00507879522309794));
#25897=CARTESIAN_POINT('Ctrl Pts',(-203.93871634638,4.9999974241789,-0.0050752536923105));
#25898=CARTESIAN_POINT('Ctrl Pts',(-203.938713709765,5.0001049778899,0.100892144113212));
#25899=CARTESIAN_POINT('Ctrl Pts',(-203.938799494166,4.99671862708652,0.206347959533171));
#25900=CARTESIAN_POINT('Ctrl Pts',(-203.938967699789,4.98996531629572,0.311310410519268));
#25901=CARTESIAN_POINT('Ctrl Pts',(-203.939138036895,4.98312642831378,0.417602933822402));
#25902=CARTESIAN_POINT('Ctrl Pts',(-203.939392912403,4.97283458317559,0.52338996686812));
#25903=CARTESIAN_POINT('Ctrl Pts',(-203.939727564256,4.95916798069977,0.628688768458106));
#25904=CARTESIAN_POINT('Ctrl Pts',(-203.940073274326,4.94504977977268,0.737467057784966));
#25905=CARTESIAN_POINT('Ctrl Pts',(-203.940504132557,4.92733017598478,0.84572488698958));
#25906=CARTESIAN_POINT('Ctrl Pts',(-203.941016241189,4.90603868496409,0.953471599031184));
#25907=CARTESIAN_POINT('Ctrl Pts',(-203.941515990555,4.88526104432011,1.0586179441695));
#25908=CARTESIAN_POINT('Ctrl Pts',(-203.942093138348,4.86108144605084,1.16327799154476));
#25909=CARTESIAN_POINT('Ctrl Pts',(-203.942745048659,4.83347748759248,1.26744392065104));
#25910=CARTESIAN_POINT('Ctrl Pts',(-203.943421142492,4.80484952178682,1.37547403021185));
#25911=CARTESIAN_POINT('Ctrl Pts',(-203.944177664023,4.77253855205537,1.48297343929525));
#25912=CARTESIAN_POINT('Ctrl Pts',(-203.945012471915,4.73646667417703,1.58990607313729));
#25913=CARTESIAN_POINT('Ctrl Pts',(-203.945800498774,4.70241619508238,1.69084640747349));
#25914=CARTESIAN_POINT('Ctrl Pts',(-203.94665830582,4.66501394975628,1.79128196025224));
#25915=CARTESIAN_POINT('Ctrl Pts',(-203.947584499091,4.62415254700364,1.89115185460711));
#25916=CARTESIAN_POINT('Ctrl Pts',(-203.94763948234,4.62172681931875,1.89708060769205));
#25917=CARTESIAN_POINT('Ctrl Pts',(-203.947694706664,4.61928888940156,1.90300735722081));
#25918=CARTESIAN_POINT('Ctrl Pts',(-203.947750171796,4.61683873043373,1.90893208653466));
#25919=CARTESIAN_POINT('Ctrl Pts',(-203.948683491776,4.57560954282768,2.00862838363326));
#25920=CARTESIAN_POINT('Ctrl Pts',(-203.949669808962,4.53153795147535,2.1062639160333));
#25921=CARTESIAN_POINT('Ctrl Pts',(-203.950699952284,4.48474857734145,2.20187922861786));
#25922=CARTESIAN_POINT('Ctrl Pts',(-203.951742583665,4.43739199240551,2.29865365134534));
#25923=CARTESIAN_POINT('Ctrl Pts',(-203.952830128236,4.38725112293232,2.39335905712821));
#25924=CARTESIAN_POINT('Ctrl Pts',(-203.953954290108,4.33440264927066,2.4860269299219));
#25925=CARTESIAN_POINT('Ctrl Pts',(-203.955118538022,4.27966967288282,2.58199920957561));
#25926=CARTESIAN_POINT('Ctrl Pts',(-203.956322077217,4.2220325491105,2.6757866843588));
#25927=CARTESIAN_POINT('Ctrl Pts',(-203.957556728966,4.16152180946428,2.76740444721753));
#25928=CARTESIAN_POINT('Ctrl Pts',(-203.958753673601,4.1028591094598,2.85622414053291));
#25929=CARTESIAN_POINT('Ctrl Pts',(-203.959979882541,4.0414951366038,2.94300498366657));
#25930=CARTESIAN_POINT('Ctrl Pts',(-203.961228553297,3.97741192006286,3.02773540654414));
#25931=CARTESIAN_POINT('Ctrl Pts',(-203.962468242802,3.91378963162541,3.11185639320373));
#25932=CARTESIAN_POINT('Ctrl Pts',(-203.963730090487,3.84748681331452,3.19395678144878));
#25933=CARTESIAN_POINT('Ctrl Pts',(-203.965007789759,3.77844536602085,3.27399396499808));
#25934=CARTESIAN_POINT('Ctrl Pts',(-203.966265184082,3.71050111200704,3.35275921316117));
#25935=CARTESIAN_POINT('Ctrl Pts',(-203.967537947166,3.63990430694283,3.42952667847006));
#25936=CARTESIAN_POINT('Ctrl Pts',(-203.968820147925,3.56656423888803,3.50421953305103));
#25937=CARTESIAN_POINT('Ctrl Pts',(-203.968983759641,3.55720588040194,3.51375051015614));
#25938=CARTESIAN_POINT('Ctrl Pts',(-203.969147524933,3.54780281043576,3.52324765428997));
#25939=CARTESIAN_POINT('Ctrl Pts',(-203.969311431355,3.53835480166774,3.53271075769229));
#25940=CARTESIAN_POINT('Ctrl Pts',(-203.969313857769,3.53821493662746,3.5328508461883));
#25941=CARTESIAN_POINT('Ctrl Pts',(-203.969316284151,3.53807506196518,3.53299092700489));
#25942=CARTESIAN_POINT('Ctrl Pts',(-203.969318710503,3.53793517768081,3.53313100014201));
#25943=CARTESIAN_POINT('Origin',(6.93889390390723E-15,1.21430643318376E-14,
12.5));
#25944=CARTESIAN_POINT('Ctrl Pts',(-203.969412573458,3.53252077317421,-3.53854447085706));
#25945=CARTESIAN_POINT('Ctrl Pts',(-203.969411275839,3.53259569826288,-3.53846967256236));
#25946=CARTESIAN_POINT('Ctrl Pts',(-203.96940997822,3.53267062140505,-3.53839487125771));
#25947=CARTESIAN_POINT('Ctrl Pts',(-203.969408680599,3.53274554260078,-3.53832006694293));
#25948=CARTESIAN_POINT('Ctrl Pts',(-203.968134468,3.60631520091507,-3.4648651811077));
#25949=CARTESIAN_POINT('Ctrl Pts',(-203.966868845506,3.67715439213078,-3.38936634640809));
#25950=CARTESIAN_POINT('Ctrl Pts',(-203.965617535976,3.74536448123347,-3.31190366563091));
#25951=CARTESIAN_POINT('Ctrl Pts',(-203.964349534112,3.81448448556256,-3.23340764105307));
#25952=CARTESIAN_POINT('Ctrl Pts',(-203.963096212182,3.88090503780374,-3.15289462678018));
#25953=CARTESIAN_POINT('Ctrl Pts',(-203.96186354839,3.94469528542177,-3.07040827976421));
#25954=CARTESIAN_POINT('Ctrl Pts',(-203.960558807129,4.01221553602298,-2.98309871396592));
#25955=CARTESIAN_POINT('Ctrl Pts',(-203.959277185763,4.07678958330119,-2.8935780934403));
#25956=CARTESIAN_POINT('Ctrl Pts',(-203.958026129452,4.13845115188194,-2.80185832588414));
#25957=CARTESIAN_POINT('Ctrl Pts',(-203.956833143225,4.19725058518819,-2.71439590026936));
#25958=CARTESIAN_POINT('Ctrl Pts',(-203.955667935116,4.25340153535253,-2.62493301863032));
#25959=CARTESIAN_POINT('Ctrl Pts',(-203.954537560927,4.30688757918469,-2.53345274735351));
#25960=CARTESIAN_POINT('Ctrl Pts',(-203.953413583761,4.36007093438034,-2.44249018194157));
#25961=CARTESIAN_POINT('Ctrl Pts',(-203.952324028895,4.41061969182416,-2.34953252211284));
#25962=CARTESIAN_POINT('Ctrl Pts',(-203.951276693114,4.4584700718099,-2.25454397745184));
#25963=CARTESIAN_POINT('Ctrl Pts',(-203.950245015845,4.50560505011277,-2.16097558796462));
#25964=CARTESIAN_POINT('Ctrl Pts',(-203.949254288028,4.55012190726754,-2.06543612011637));
#25965=CARTESIAN_POINT('Ctrl Pts',(-203.948313055999,4.59191045159328,-1.9678797168031));
#25966=CARTESIAN_POINT('Ctrl Pts',(-203.948147566562,4.59925780322778,-1.95072714039958));
#25967=CARTESIAN_POINT('Ctrl Pts',(-203.947983610346,4.60652068476313,-1.93351219424609));
#25968=CARTESIAN_POINT('Ctrl Pts',(-203.94782123798,4.613698330089,-1.91623460785442));
#25969=CARTESIAN_POINT('Ctrl Pts',(-203.946900124353,4.65441601552921,-1.81822149966598));
#25970=CARTESIAN_POINT('Ctrl Pts',(-203.946045172056,4.69176958275255,-1.71969832859259));
#25971=CARTESIAN_POINT('Ctrl Pts',(-203.945257471353,4.72587584163911,-1.62071281896581));
#25972=CARTESIAN_POINT('Ctrl Pts',(-203.944460536852,4.76038191014495,-1.52056695460618));
#25973=CARTESIAN_POINT('Ctrl Pts',(-203.943732421809,4.7915643076881,-1.41994737344693));
#25974=CARTESIAN_POINT('Ctrl Pts',(-203.943074663623,4.81950096756316,-1.31887158134935));
#25975=CARTESIAN_POINT('Ctrl Pts',(-203.942413007084,4.84760320038007,-1.21719674067824));
#25976=CARTESIAN_POINT('Ctrl Pts',(-203.941822525777,4.87242131004307,-1.11505977428861));
#25977=CARTESIAN_POINT('Ctrl Pts',(-203.941305468174,4.8939882340887,-1.01245374825097));
#25978=CARTESIAN_POINT('Ctrl Pts',(-203.940789741936,4.91549962575811,-0.910111921059155));
#25979=CARTESIAN_POINT('Ctrl Pts',(-203.940347044837,4.93377671234906,-0.807302952881646));
#25980=CARTESIAN_POINT('Ctrl Pts',(-203.939980546822,4.94880355906628,-0.704002840896675));
#25981=CARTESIAN_POINT('Ctrl Pts',(-203.939616664476,4.96372316028913,-0.601439974175979));
#25982=CARTESIAN_POINT('Ctrl Pts',(-203.93932788155,4.97543889374863,-0.498392480078721));
#25983=CARTESIAN_POINT('Ctrl Pts',(-203.939118470203,4.98388497402619,-0.394827141948199));
#25984=CARTESIAN_POINT('Ctrl Pts',(-203.938912457629,4.99219397340393,-0.292942681724858));
#25985=CARTESIAN_POINT('Ctrl Pts',(-203.938783247807,4.99733867728785,-0.190556617638261));
#25986=CARTESIAN_POINT('Ctrl Pts',(-203.938736256528,4.99920612957307,-0.0876345386283712));
#25987=CARTESIAN_POINT('Ctrl Pts',(-203.938723723722,4.99970418832119,-0.0601847118080584));
#25988=CARTESIAN_POINT('Ctrl Pts',(-203.938717047394,4.9999688458647,-0.0326967616464312));
#25989=CARTESIAN_POINT('Ctrl Pts',(-203.938716348762,4.99999732701828,-0.00517006110607632));
#25990=CARTESIAN_POINT('Origin',(6.93889390390723E-15,1.21430643318376E-14,
12.5));
#25991=CARTESIAN_POINT('Ctrl Pts',(-203.999999998715,-4.1209657214436E-14,
-4.99999998173599));
#25992=CARTESIAN_POINT('Ctrl Pts',(-203.999999851572,0.101478108507438,
-4.99999789027357));
#25993=CARTESIAN_POINT('Ctrl Pts',(-203.999911491604,0.202547192110731,
-4.99673137395367));
#25994=CARTESIAN_POINT('Ctrl Pts',(-203.999742496303,0.303223851399144,
-4.99032853877155));
#25995=CARTESIAN_POINT('Ctrl Pts',(-203.999570703464,0.405567105534984,
-4.9838197114737));
#25996=CARTESIAN_POINT('Ctrl Pts',(-203.999315569935,0.507505311344336,
-4.97406977581446));
#25997=CARTESIAN_POINT('Ctrl Pts',(-203.998983564952,0.60905786453182,-4.96115979848574));
#25998=CARTESIAN_POINT('Ctrl Pts',(-203.998647122097,0.711967858954138,
-4.94807725498299));
#25999=CARTESIAN_POINT('Ctrl Pts',(-203.998231724043,0.814482346588999,
-4.93174952421542));
#26000=CARTESIAN_POINT('Ctrl Pts',(-203.997742803152,0.916615882329558,
-4.91220799556483));
#26001=CARTESIAN_POINT('Ctrl Pts',(-203.997253924647,1.01874056404149,-4.89266816098322));
#26002=CARTESIAN_POINT('Ctrl Pts',(-203.996691518543,1.12048489244614,-4.8699148964471));
#26003=CARTESIAN_POINT('Ctrl Pts',(-203.996059973582,1.22184988589826,-4.84392933565863));
#26004=CARTESIAN_POINT('Ctrl Pts',(-203.995432907184,1.32249605576609,-4.81812804986796));
#26005=CARTESIAN_POINT('Ctrl Pts',(-203.994737661213,1.42276877071541,-4.78913993588124));
#26006=CARTESIAN_POINT('Ctrl Pts',(-203.993977768997,1.52264788095545,-4.75690006435692));
#26007=CARTESIAN_POINT('Ctrl Pts',(-203.993228127426,1.62117966161722,-4.72509509591093));
#26008=CARTESIAN_POINT('Ctrl Pts',(-203.992415554537,1.71932887167901,-4.69012528273805));
#26009=CARTESIAN_POINT('Ctrl Pts',(-203.991542958962,1.81704812208673,-4.65188621442636));
#26010=CARTESIAN_POINT('Ctrl Pts',(-203.991352020189,1.83843075833679,-4.6435188550285));
#26011=CARTESIAN_POINT('Ctrl Pts',(-203.991158206183,1.85979268381466,-4.6349948061121));
#26012=CARTESIAN_POINT('Ctrl Pts',(-203.990961545547,1.88113318328502,-4.62631271594245));
#26013=CARTESIAN_POINT('Ctrl Pts',(-203.990885740832,1.88935908201384,-4.62296612161418));
#26014=CARTESIAN_POINT('Ctrl Pts',(-203.990809513162,1.89758179638646,-4.61959604470624));
#26015=CARTESIAN_POINT('Ctrl Pts',(-203.990732864159,1.90580128199572,-4.61620240419527));
#26016=CARTESIAN_POINT('Ctrl Pts',(-203.990664473972,1.91313513024385,-4.61317442340677));
#26017=CARTESIAN_POINT('Ctrl Pts',(-203.990595782027,1.92046277100155,-4.61012917130543));
#26018=CARTESIAN_POINT('Ctrl Pts',(-203.990526862118,1.92777665320724,-4.60706983383067));
#26019=CARTESIAN_POINT('Ctrl Pts',(-203.98961484747,2.02456099013266,-4.56658573241935));
#26020=CARTESIAN_POINT('Ctrl Pts',(-203.988659330757,2.11933307478242,-4.52347601725412));
#26021=CARTESIAN_POINT('Ctrl Pts',(-203.987667121574,2.21213936003649,-4.47785962810522));
#26022=CARTESIAN_POINT('Ctrl Pts',(-203.986663494819,2.30601358783902,-4.43171832102921));
#26023=CARTESIAN_POINT('Ctrl Pts',(-203.985622308448,2.39787702616031,-4.38301209941167));
#26024=CARTESIAN_POINT('Ctrl Pts',(-203.984549391421,2.48776893667968,-4.33181135199818));
#26025=CARTESIAN_POINT('Ctrl Pts',(-203.983467856286,2.57838289563658,-4.28019933932782));
#26026=CARTESIAN_POINT('Ctrl Pts',(-203.982354060498,2.66699405089007,-4.22605234310404));
#26027=CARTESIAN_POINT('Ctrl Pts',(-203.981213017644,2.75362587927287,-4.16939260747491));
#26028=CARTESIAN_POINT('Ctrl Pts',(-203.981096128022,2.76250053427264,-4.16358832496728));
#26029=CARTESIAN_POINT('Ctrl Pts',(-203.980978951783,2.7713543994495,-4.15775763221893));
#26030=CARTESIAN_POINT('Ctrl Pts',(-203.980861493872,2.78018748681088,-4.15190052529389));
#26031=CARTESIAN_POINT('Ctrl Pts',(-203.979859088338,2.85557053765398,-4.10191499123766));
#26032=CARTESIAN_POINT('Ctrl Pts',(-203.978837504642,2.92934542439754,-4.05007367992567));
#26033=CARTESIAN_POINT('Ctrl Pts',(-203.977798594993,3.00159775461004,-3.99631196514068));
#26034=CARTESIAN_POINT('Ctrl Pts',(-203.976767279042,3.07332197106984,-3.94294321070539));
#26035=CARTESIAN_POINT('Ctrl Pts',(-203.975718873857,3.14354620234686,-3.88768178534922));
#26036=CARTESIAN_POINT('Ctrl Pts',(-203.974654798023,3.21232371174674,-3.83042363989903));
#26037=CARTESIAN_POINT('Ctrl Pts',(-203.973610516975,3.27982176716291,-3.77423065605377));
#26038=CARTESIAN_POINT('Ctrl Pts',(-203.972551128472,3.34592674794902,-3.71611429378542));
#26039=CARTESIAN_POINT('Ctrl Pts',(-203.971477814882,3.4106543595515,-3.65594048143801));
#26040=CARTESIAN_POINT('Ctrl Pts',(-203.970797314893,3.45169282156614,-3.61778920949765));
#26041=CARTESIAN_POINT('Ctrl Pts',(-203.970111214813,3.49217690578241,-3.57881018648497));
#26042=CARTESIAN_POINT('Ctrl Pts',(-203.969419821476,3.53210224850348,-3.53896223575735));
#26043=CARTESIAN_POINT('Ctrl Pts',(-203.969417405474,3.53224176347508,-3.53882299122405));
#26044=CARTESIAN_POINT('Ctrl Pts',(-203.969414989468,3.53238127169852,-3.53868373625768));
#26045=CARTESIAN_POINT('Ctrl Pts',(-203.969412573458,3.53252077317421,-3.53854447085706));
#26046=CARTESIAN_POINT('Origin',(6.93889390390723E-15,1.21430643318376E-14,
12.5));
#26047=CARTESIAN_POINT('Ctrl Pts',(-203.969331848638,-3.53718156034075,
-3.53388548308073));
#26048=CARTESIAN_POINT('Ctrl Pts',(-203.96933263622,-3.53713614484727,-3.53393094079166));
#26049=CARTESIAN_POINT('Ctrl Pts',(-203.969333423798,-3.53709072838883,
-3.53397639765148));
#26050=CARTESIAN_POINT('Ctrl Pts',(-203.969334211371,-3.53704531096541,
-3.53402185366019));
#26051=CARTESIAN_POINT('Ctrl Pts',(-203.970636762969,-3.46193033865401,
-3.60920064143309));
#26052=CARTESIAN_POINT('Ctrl Pts',(-203.971924002428,-3.38470365609248,
-3.68152944605214));
#26053=CARTESIAN_POINT('Ctrl Pts',(-203.97319187132,-3.30544129092278,-3.75111104527892));
#26054=CARTESIAN_POINT('Ctrl Pts',(-203.974475554871,-3.22519025314963,
-3.82156056487008));
#26055=CARTESIAN_POINT('Ctrl Pts',(-203.975739398606,-3.14285202075756,
-3.88919414923696));
#26056=CARTESIAN_POINT('Ctrl Pts',(-203.976979043182,-3.05846905612516,
-3.95407910561204));
#26057=CARTESIAN_POINT('Ctrl Pts',(-203.978255220119,-2.97159932320146,
-4.02087622343817));
#26058=CARTESIAN_POINT('Ctrl Pts',(-203.979505771654,-2.8825621978443,-4.08476074195069));
#26059=CARTESIAN_POINT('Ctrl Pts',(-203.980725493441,-2.7913714701466,-4.14575947632592));
#26060=CARTESIAN_POINT('Ctrl Pts',(-203.981919492977,-2.70210382915404,
-4.20547183150373));
#26061=CARTESIAN_POINT('Ctrl Pts',(-203.983083965809,-2.61077188188111,
-4.26241888838065));
#26062=CARTESIAN_POINT('Ctrl Pts',(-203.984213332899,-2.51736531855809,
-4.31657884047884));
#26063=CARTESIAN_POINT('Ctrl Pts',(-203.985379194806,-2.42094037839488,
-4.37248893881155));
#26064=CARTESIAN_POINT('Ctrl Pts',(-203.98650767288,-2.32230412745077,-4.42542946900403));
#26065=CARTESIAN_POINT('Ctrl Pts',(-203.98759153748,-2.22142770237638,-4.47532051437978));
#26066=CARTESIAN_POINT('Ctrl Pts',(-203.988619493194,-2.12575477637829,
-4.52263803468924));
#26067=CARTESIAN_POINT('Ctrl Pts',(-203.989607328797,-2.02806626724635,
-4.5672123814815));
#26068=CARTESIAN_POINT('Ctrl Pts',(-203.990547667339,-1.92832974439805,
-4.60892427326972));
#26069=CARTESIAN_POINT('Ctrl Pts',(-203.990598810864,-1.92290523271829,
-4.61119291706969));
#26070=CARTESIAN_POINT('Ctrl Pts',(-203.990649813556,-1.91747466197154,
-4.61345308059517));
#26071=CARTESIAN_POINT('Ctrl Pts',(-203.990700674109,-1.91203802672089,
-4.61570474017852));
#26072=CARTESIAN_POINT('Ctrl Pts',(-203.991624460392,-1.8132917723089,-4.65660190171607));
#26073=CARTESIAN_POINT('Ctrl Pts',(-203.992487633228,-1.71401719948977,
-4.69408846950362));
#26074=CARTESIAN_POINT('Ctrl Pts',(-203.993287114536,-1.61426436199689,
-4.72828343912112));
#26075=CARTESIAN_POINT('Ctrl Pts',(-203.994094953937,-1.51346866902538,
-4.76283589642822));
#26076=CARTESIAN_POINT('Ctrl Pts',(-203.994837780494,-1.41218417208542,
-4.79402774654659));
#26077=CARTESIAN_POINT('Ctrl Pts',(-203.995511933048,-1.31043346085766,
-4.8219370383235));
#26078=CARTESIAN_POINT('Ctrl Pts',(-203.996191074818,-1.20792972070238,
-4.85005287906505));
#26079=CARTESIAN_POINT('Ctrl Pts',(-203.996800540141,-1.10495234407624,
-4.8748375765012));
#26080=CARTESIAN_POINT('Ctrl Pts',(-203.997335830203,-1.00150255967545,
-4.89632312555432));
#26081=CARTESIAN_POINT('Ctrl Pts',(-203.997390348359,-0.990966418640601,
-4.89851138313596));
#26082=CARTESIAN_POINT('Ctrl Pts',(-203.997444096318,-0.98042536252555,
-4.90066537665444));
#26083=CARTESIAN_POINT('Ctrl Pts',(-203.997497068777,-0.969879383161346,
-4.90278511114707));
#26084=CARTESIAN_POINT('Ctrl Pts',(-203.998675482326,-0.735275867146641,
-4.94994025414655));
#26085=CARTESIAN_POINT('Ctrl Pts',(-203.999475416986,-0.497158016437222,
-4.98036087920727));
#26086=CARTESIAN_POINT('Ctrl Pts',(-203.99981546314,-0.257667439114993,
-4.99312496300635));
#26087=CARTESIAN_POINT('Ctrl Pts',(-203.999936376277,-0.172509714040374,
-4.99766359810066));
#26088=CARTESIAN_POINT('Ctrl Pts',(-203.999999125432,-0.0871786927026717,
-4.99996942432042));
#26089=CARTESIAN_POINT('Ctrl Pts',(-203.999999989755,-0.00177162224212113,
-4.99999968613545));
#26090=CARTESIAN_POINT('Ctrl Pts',(-203.999999992743,-0.0014763523465126,
-4.9999997907568));
#26091=CARTESIAN_POINT('Ctrl Pts',(-203.999999994983,-0.00118108191426726,
-4.99999986769981));
#26092=CARTESIAN_POINT('Ctrl Pts',(-203.999999996477,-0.000885810949727572,
-4.99999991696603));
#26093=CARTESIAN_POINT('Origin',(6.93889390390723E-15,1.21430643318376E-14,
12.5));
#26094=CARTESIAN_POINT('Ctrl Pts',(-203.938716194739,-4.99999958112187,
0.00204287664667743));
#26095=CARTESIAN_POINT('Ctrl Pts',(-203.938715152034,-5.0000417830682,-0.102528719030479));
#26096=CARTESIAN_POINT('Ctrl Pts',(-203.938800539213,-4.99667457281812,
-0.206607538294783));
#26097=CARTESIAN_POINT('Ctrl Pts',(-203.938966293367,-4.99002608380757,
-0.310206534216836));
#26098=CARTESIAN_POINT('Ctrl Pts',(-203.939134229435,-4.98329007704069,
-0.415169261306567));
#26099=CARTESIAN_POINT('Ctrl Pts',(-203.939384676877,-4.9731857396949,-0.519639916075042));
#26100=CARTESIAN_POINT('Ctrl Pts',(-203.93971286547,-4.95979262703873,-0.623634161057456));
#26101=CARTESIAN_POINT('Ctrl Pts',(-203.940057644038,-4.94572249081783,
-0.732885328478902));
#26102=CARTESIAN_POINT('Ctrl Pts',(-203.940488230322,-4.92802295076255,
-0.841611316229411));
#26103=CARTESIAN_POINT('Ctrl Pts',(-203.941000611062,-4.90672556926535,
-0.949824308092555));
#26104=CARTESIAN_POINT('Ctrl Pts',(-203.941492763979,-4.88626896810742,
-1.0537652557129));
#26105=CARTESIAN_POINT('Ctrl Pts',(-203.942060406374,-4.86249247252813,
-1.15723335870826));
#26106=CARTESIAN_POINT('Ctrl Pts',(-203.94270105974,-4.83537271866045,-1.26022634082892));
#26107=CARTESIAN_POINT('Ctrl Pts',(-203.94333810678,-4.80840562560068,-1.36263956135086));
#26108=CARTESIAN_POINT('Ctrl Pts',(-203.944047362564,-4.77813263765291,
-1.46458349161457));
#26109=CARTESIAN_POINT('Ctrl Pts',(-203.944827171486,-4.74448357436985,
-1.56603569119861));
#26110=CARTESIAN_POINT('Ctrl Pts',(-203.945595488905,-4.71133037405031,
-1.66599285991305));
#26111=CARTESIAN_POINT('Ctrl Pts',(-203.946432312624,-4.67489966245849,
-1.76547313517111));
#26112=CARTESIAN_POINT('Ctrl Pts',(-203.947336562213,-4.63508122875481,
-1.86442843748819));
#26113=CARTESIAN_POINT('Ctrl Pts',(-203.947474281927,-4.62901677113549,
-1.87949960381216));
#26114=CARTESIAN_POINT('Ctrl Pts',(-203.947613566339,-4.6228736522463,-1.89455853425889));
#26115=CARTESIAN_POINT('Ctrl Pts',(-203.947754412286,-4.61665139773073,
-1.90960499330604));
#26116=CARTESIAN_POINT('Ctrl Pts',(-203.948679171294,-4.57579764205161,
-2.00839625300285));
#26117=CARTESIAN_POINT('Ctrl Pts',(-203.949656115491,-4.5321554336636,-2.10515411801173));
#26118=CARTESIAN_POINT('Ctrl Pts',(-203.950676240678,-4.48584283790299,
-2.19992344521772));
#26119=CARTESIAN_POINT('Ctrl Pts',(-203.951708300859,-4.43898840613736,
-2.29580152983209));
#26120=CARTESIAN_POINT('Ctrl Pts',(-203.952784575849,-4.38940055633292,
-2.38964476280578));
#26121=CARTESIAN_POINT('Ctrl Pts',(-203.953897000685,-4.3371485721777,-2.48149181013575));
#26122=CARTESIAN_POINT('Ctrl Pts',(-203.955064903076,-4.28229073797331,
-2.57791934635375));
#26123=CARTESIAN_POINT('Ctrl Pts',(-203.956272663953,-4.22449658832434,
-2.67214732123704));
#26124=CARTESIAN_POINT('Ctrl Pts',(-203.957512102244,-4.16378789801569,
-2.76420269877084));
#26125=CARTESIAN_POINT('Ctrl Pts',(-203.958696582427,-4.10577110031478,
-2.85217623581319));
#26126=CARTESIAN_POINT('Ctrl Pts',(-203.95991001783,-4.04509190437419,-2.93816590008804));
#26127=CARTESIAN_POINT('Ctrl Pts',(-203.961145986998,-3.98172187707493,
-3.02217234792129));
#26128=CARTESIAN_POINT('Ctrl Pts',(-203.962373099065,-3.91880596694053,
-3.10557679554172));
#26129=CARTESIAN_POINT('Ctrl Pts',(-203.963622440477,-3.85323742532754,
-3.18702678160715));
#26130=CARTESIAN_POINT('Ctrl Pts',(-203.964888151834,-3.78494613139692,
-3.26649414243936));
#26131=CARTESIAN_POINT('Ctrl Pts',(-203.966133891314,-3.71773241754321,
-3.34470757411209));
#26132=CARTESIAN_POINT('Ctrl Pts',(-203.967395504321,-3.64788095752727,
-3.42100082378285));
#26133=CARTESIAN_POINT('Ctrl Pts',(-203.968667570102,-3.57528732430931,
-3.49531319775564));
#26134=CARTESIAN_POINT('Ctrl Pts',(-203.968887824704,-3.56271794143041,
-3.50818017574942));
#26135=CARTESIAN_POINT('Ctrl Pts',(-203.96910839275,-3.5500662608768,-3.52098767609423));
#26136=CARTESIAN_POINT('Ctrl Pts',(-203.969329246069,-3.53733163160961,
-3.53373526569466));
#26137=CARTESIAN_POINT('Ctrl Pts',(-203.969330113598,-3.5372816090241,-3.53378533918933));
#26138=CARTESIAN_POINT('Ctrl Pts',(-203.969330981121,-3.53723158526782,
-3.53383541165135));
#26139=CARTESIAN_POINT('Ctrl Pts',(-203.969331848638,-3.53718156034075,
-3.53388548308073));
#26140=CARTESIAN_POINT('Origin',(-6.93889390390723E-15,1.21430643318376E-14,
7.));
#26141=CARTESIAN_POINT('',(184.50486486776,-91.6185289127127,7.));
#26142=CARTESIAN_POINT('',(184.50486486776,91.6185289127127,7.));
#26143=CARTESIAN_POINT('Origin',(-6.93889390390723E-15,1.21430643318376E-14,
7.));
#26144=CARTESIAN_POINT('',(184.50486486776,91.6185289127127,10.));
#26145=CARTESIAN_POINT('',(184.50486486776,91.6185289127127,7.));
#26146=CARTESIAN_POINT('',(184.50486486776,-91.6185289127127,10.));
#26147=CARTESIAN_POINT('Origin',(-6.93889390390723E-15,1.21430643318376E-14,
10.));
#26148=CARTESIAN_POINT('',(184.50486486776,-91.6185289127127,7.));
#26149=CARTESIAN_POINT('Origin',(71.5953323638214,6.93889390390723E-15,
7.));
#26150=CARTESIAN_POINT('Origin',(71.5953323638214,6.93889390390723E-15,
7.));
#26151=CARTESIAN_POINT('Origin',(71.5953323638214,6.93889390390723E-15,
10.));
#26152=CARTESIAN_POINT('Origin',(210.,0.,0.));
#26153=CARTESIAN_POINT('',(210.,-6.12323399573677E-16,-5.));
#26154=CARTESIAN_POINT('Origin',(210.,0.,0.));
#26155=CARTESIAN_POINT('',(204.000000000871,-0.000351443158057461,-4.9999996843097));
#26156=CARTESIAN_POINT('',(210.,-6.12323399573677E-16,-5.));
#26157=CARTESIAN_POINT('',(203.969329275182,-3.53733162599185,-3.53373527131814));
#26158=CARTESIAN_POINT('Ctrl Pts',(203.969329275182,-3.53733162599185,-3.53373527131814));
#26159=CARTESIAN_POINT('Ctrl Pts',(203.969339665773,-3.53673248458769,-3.53433502248076));
#26160=CARTESIAN_POINT('Ctrl Pts',(203.969350055435,-3.53613324448486,-3.53493456738062));
#26161=CARTESIAN_POINT('Ctrl Pts',(203.977055116563,-3.09161865850825,-3.97944915335723));
#26162=CARTESIAN_POINT('Ctrl Pts',(203.985248421744,-2.52939665845125,-4.36424514979789));
#26163=CARTESIAN_POINT('Ctrl Pts',(203.996801483377,-1.29773742182364,-4.87442600971193));
#26164=CARTESIAN_POINT('Ctrl Pts',(203.999997835124,-0.628338172338108,
-4.99991167307061));
#26165=CARTESIAN_POINT('Ctrl Pts',(203.999999998788,-0.000703254944229431,
-4.99999995054325));
#26166=CARTESIAN_POINT('',(203.938716302406,-4.99999929267631,0.00265955567476925));
#26167=CARTESIAN_POINT('Ctrl Pts',(203.938716302406,-4.99999929267631,0.00265955567477076));
#26168=CARTESIAN_POINT('Ctrl Pts',(203.938716290844,-4.99999976426973,0.00177295390105103));
#26169=CARTESIAN_POINT('Ctrl Pts',(203.938716285064,-5.,0.000886435252659898));
#26170=CARTESIAN_POINT('Ctrl Pts',(203.938716285064,-5.,-0.627838125135884));
#26171=CARTESIAN_POINT('Ctrl Pts',(203.941913718727,-4.87452126623505,-1.29750745448768));
#26172=CARTESIAN_POINT('Ctrl Pts',(203.953463590422,-4.36458961878151,-2.52856505718217));
#26173=CARTESIAN_POINT('Ctrl Pts',(203.961643611968,-3.98050171479364,-3.09011415925124));
#26174=CARTESIAN_POINT('Ctrl Pts',(203.969329275182,-3.53733162599185,-3.53373527131814));
#26175=CARTESIAN_POINT('',(203.969357682308,-3.53569323348296,3.53537456396855));
#26176=CARTESIAN_POINT('Ctrl Pts',(203.969354900228,-3.535853727891,3.53521405504098));
#26177=CARTESIAN_POINT('Ctrl Pts',(203.961661829301,-3.97963642785498,3.09135105562694));
#26178=CARTESIAN_POINT('Ctrl Pts',(203.953470004699,-4.36430642577637,2.52924873097206));
#26179=CARTESIAN_POINT('Ctrl Pts',(203.94192187778,-4.87416104063058,1.29837709745118));
#26180=CARTESIAN_POINT('Ctrl Pts',(203.938724479991,-4.99966574739792,0.629729021401888));
#26181=CARTESIAN_POINT('Ctrl Pts',(203.938716302406,-4.99999929267631,0.00265955567477064));
#26182=CARTESIAN_POINT('',(204.,1.86713497344704E-14,5.));
#26183=CARTESIAN_POINT('Ctrl Pts',(204.,2.77555756156289E-16,5.));
#26184=CARTESIAN_POINT('Ctrl Pts',(204.,-0.627838117491495,5.));
#26185=CARTESIAN_POINT('Ctrl Pts',(203.996803640531,-1.29750744995471,4.8745212692142));
#26186=CARTESIAN_POINT('Ctrl Pts',(203.985248421744,-2.52939665845125,4.36424514979789));
#26187=CARTESIAN_POINT('Ctrl Pts',(203.977055116563,-3.09161865850825,3.97944915335723));
#26188=CARTESIAN_POINT('Ctrl Pts',(203.969360444161,-3.53553390593274,3.53553390593274));
#26189=CARTESIAN_POINT('',(203.969311528224,3.5383548016686,3.53271075769143));
#26190=CARTESIAN_POINT('Ctrl Pts',(203.969311528224,3.5383548016686,3.53271075769143));
#26191=CARTESIAN_POINT('Ctrl Pts',(203.969327835823,3.53741474617601,3.53365231506597));
#26192=CARTESIAN_POINT('Ctrl Pts',(203.969344141145,3.53647444727618,3.53459336458929));
#26193=CARTESIAN_POINT('Ctrl Pts',(203.977055116563,3.09161865850825,3.97944915335723));
#26194=CARTESIAN_POINT('Ctrl Pts',(203.985248421744,2.52939665845125,4.36424514979789));
#26195=CARTESIAN_POINT('Ctrl Pts',(203.996803640531,1.29750744995471,4.8745212692142));
#26196=CARTESIAN_POINT('Ctrl Pts',(204.,0.627838117491496,5.));
#26197=CARTESIAN_POINT('Ctrl Pts',(204.,2.77555756156289E-16,5.));
#26198=CARTESIAN_POINT('',(203.938716348481,4.99999741338323,-0.00508587858850655));
#26199=CARTESIAN_POINT('Ctrl Pts',(203.938716348481,4.99999741338323,-0.00508587858850455));
#26200=CARTESIAN_POINT('Ctrl Pts',(203.938716306196,4.99999913810376,-0.00339028203939836));
#26201=CARTESIAN_POINT('Ctrl Pts',(203.938716285064,5.,-0.00169498854628657));
#26202=CARTESIAN_POINT('Ctrl Pts',(203.938716285064,5.,0.));
#26203=CARTESIAN_POINT('Ctrl Pts',(203.938716285064,5.,0.627838125135885));
#26204=CARTESIAN_POINT('Ctrl Pts',(203.941913718727,4.87452126623505,1.29750745448768));
#26205=CARTESIAN_POINT('Ctrl Pts',(203.953459148684,4.36478572336839,2.52809162894172));
#26206=CARTESIAN_POINT('Ctrl Pts',(203.961631000106,3.98110068786657,3.08925751744615));
#26207=CARTESIAN_POINT('Ctrl Pts',(203.969311528224,3.5383548016686,3.53271075769143));
#26208=CARTESIAN_POINT('',(203.96941989844,3.5321022485035,-3.53896223575733));
#26209=CARTESIAN_POINT('Ctrl Pts',(203.96941989844,3.5321022485035,-3.53896223575733));
#26210=CARTESIAN_POINT('Ctrl Pts',(203.96940007698,3.53324688460997,-3.53781981843381));
#26211=CARTESIAN_POINT('Ctrl Pts',(203.969380258871,3.53439077061651,-3.53667704124896));
#26212=CARTESIAN_POINT('Ctrl Pts',(203.961665771665,3.97944915876222,-3.09161865310326));
#26213=CARTESIAN_POINT('Ctrl Pts',(203.953471392542,4.36424515196542,-2.52939665587767));
#26214=CARTESIAN_POINT('Ctrl Pts',(203.941929319981,4.87383246434926,-1.29917033382159));
#26215=CARTESIAN_POINT('Ctrl Pts',(203.938731969008,4.9993602870002,-0.631453616573415));
#26216=CARTESIAN_POINT('Ctrl Pts',(203.938716348481,4.99999741338323,-0.00508587858850454));
#26217=CARTESIAN_POINT('Ctrl Pts',(204.,-4.16333634234434E-16,-5.));
#26218=CARTESIAN_POINT('Ctrl Pts',(204.,0.627838117491495,-5.));
#26219=CARTESIAN_POINT('Ctrl Pts',(203.996803640531,1.29750744995471,-4.8745212692142));
#26220=CARTESIAN_POINT('Ctrl Pts',(203.985263299786,2.52781052678752,-4.3649021610816));
#26221=CARTESIAN_POINT('Ctrl Pts',(203.977097370854,3.08874883332667,-3.98145624679971));
#26222=CARTESIAN_POINT('Ctrl Pts',(203.96941989844,3.5321022485035,-3.53896223575733));
#26223=CARTESIAN_POINT('Origin',(71.5953323638214,6.93889390390723E-15,
-10.));
#26224=CARTESIAN_POINT('',(174.6884520924,105.356275112407,-10.));
#26225=CARTESIAN_POINT('',(174.6884520924,-105.356275112407,-10.));
#26226=CARTESIAN_POINT('Origin',(71.5953323638214,6.93889390390723E-15,
-10.));
#26227=CARTESIAN_POINT('',(174.6884520924,105.356275112407,10.));
#26228=CARTESIAN_POINT('',(174.6884520924,105.356275112407,-10.));
#26229=CARTESIAN_POINT('',(174.6884520924,-105.356275112407,10.));
#26230=CARTESIAN_POINT('Origin',(71.5953323638214,6.93889390390723E-15,
10.));
#26231=CARTESIAN_POINT('',(174.6884520924,-105.356275112407,-10.));
#26232=CARTESIAN_POINT('Origin',(35.7976661819107,9.54097911787244E-15,
10.));
#26233=CARTESIAN_POINT('',(204.,-1.28397303707684E-14,10.));
#26234=CARTESIAN_POINT('Origin',(6.93889390390723E-15,1.21430643318376E-14,
10.));
#26235=CARTESIAN_POINT('Origin',(6.93889390390723E-15,1.21430643318376E-14,
10.));
#26236=CARTESIAN_POINT('Origin',(35.7976661819107,9.54097911787244E-15,
-10.));
#26237=CARTESIAN_POINT('',(204.,-1.28397303707684E-14,-10.));
#26238=CARTESIAN_POINT('Origin',(6.93889390390723E-15,1.21430643318376E-14,
-10.));
#26239=CARTESIAN_POINT('Origin',(6.93889390390723E-15,1.21430643318376E-14,
-10.));
#26240=CARTESIAN_POINT('',(184.50486486776,91.6185289127127,-10.));
#26241=CARTESIAN_POINT('',(184.50486486776,-91.6185289127127,-10.));
#26242=CARTESIAN_POINT('Origin',(71.5953323638214,6.93889390390723E-15,
-10.));
#26243=CARTESIAN_POINT('Origin',(-6.93889390390723E-15,1.21430643318376E-14,
-10.));
#26244=CARTESIAN_POINT('Origin',(210.,0.,0.));
#26245=CARTESIAN_POINT('Origin',(71.5953323638214,6.93889390390723E-15,
-7.));
#26246=CARTESIAN_POINT('',(184.50486486776,-91.6185289127127,-7.));
#26247=CARTESIAN_POINT('',(184.50486486776,-91.6185289127127,-7.));
#26248=CARTESIAN_POINT('',(184.50486486776,91.6185289127127,-7.));
#26249=CARTESIAN_POINT('Origin',(71.5953323638214,6.93889390390723E-15,
-7.));
#26250=CARTESIAN_POINT('',(184.50486486776,91.6185289127127,-7.));
#26251=CARTESIAN_POINT('Origin',(-6.93889390390723E-15,1.21430643318376E-14,
-7.));
#26252=CARTESIAN_POINT('Origin',(-6.93889390390723E-15,1.21430643318376E-14,
-7.));
#26253=CARTESIAN_POINT('Origin',(35.7976661819107,9.54097911787244E-15,
-7.));
#26254=CARTESIAN_POINT('Origin',(35.7976661819107,9.54097911787244E-15,
7.));
#26255=CARTESIAN_POINT('Origin',(6.93889390390723E-15,1.21430643318376E-14,
12.5));
#26256=CARTESIAN_POINT('Ctrl Pts',(203.969311528224,3.53835480166773,3.5327107576923));
#26257=CARTESIAN_POINT('Ctrl Pts',(203.985313878591,2.61589547515511,4.45664385360227));
#26258=CARTESIAN_POINT('Ctrl Pts',(204.,1.32135029102454,5.));
#26259=CARTESIAN_POINT('Ctrl Pts',(204.,1.86713497344704E-14,5.));
#26260=CARTESIAN_POINT('Origin',(6.93889390390723E-15,1.21430643318376E-14,
12.5));
#26261=CARTESIAN_POINT('Ctrl Pts',(204.,1.86713497344704E-14,5.));
#26262=CARTESIAN_POINT('Ctrl Pts',(204.,-1.32135029102454,5.));
#26263=CARTESIAN_POINT('Ctrl Pts',(203.985345962115,-2.61339289425715,4.45784180166547));
#26264=CARTESIAN_POINT('Ctrl Pts',(203.969354900227,-3.535853727891,3.53521405504098));
#26265=CARTESIAN_POINT('Origin',(6.93889390390723E-15,1.21430643318376E-14,
12.5));
#26266=CARTESIAN_POINT('Ctrl Pts',(203.969354900227,-3.535853727891,3.53521405504098));
#26267=CARTESIAN_POINT('Ctrl Pts',(203.95336383834,-4.45831456152485,2.61258630841649));
#26268=CARTESIAN_POINT('Ctrl Pts',(203.938733312599,-4.99930548519226,1.30702665821117));
#26269=CARTESIAN_POINT('Ctrl Pts',(203.938716302406,-4.99999929267631,0.00265955567476928));
#26270=CARTESIAN_POINT('Origin',(6.93889390390723E-15,1.21430643318376E-14,
12.5));
#26271=CARTESIAN_POINT('Ctrl Pts',(203.938716302406,-4.99999929267631,0.00265955567476928));
#26272=CARTESIAN_POINT('Ctrl Pts',(203.938699292213,-5.00069310016037,-1.30170754686164));
#26273=CARTESIAN_POINT('Ctrl Pts',(203.953150206634,-4.47024776275284,-2.59986968375128));
#26274=CARTESIAN_POINT('Ctrl Pts',(203.969329275085,-3.5373316316096,-3.53373526569467));
#26275=CARTESIAN_POINT('Origin',(6.93889390390723E-15,1.21430643318376E-14,
12.5));
#26276=CARTESIAN_POINT('Ctrl Pts',(203.969329275182,-3.53733162599185,-3.53373527131814));
#26277=CARTESIAN_POINT('Ctrl Pts',(203.985508343594,-2.60441549525788,-4.4676008497735));
#26278=CARTESIAN_POINT('Ctrl Pts',(203.99998865724,-1.30698993165052,-4.99953721534887));
#26279=CARTESIAN_POINT('Ctrl Pts',(203.999999994872,-0.0014763518149245,
-4.99999979075699));
#26280=CARTESIAN_POINT('Ctrl Pts',(203.999999996688,-0.0011810813606895,
-4.9999998676999));
#26281=CARTESIAN_POINT('Ctrl Pts',(203.999999997836,-0.000885810883897428,
-4.9999999180906));
#26282=CARTESIAN_POINT('Origin',(6.93889390390723E-15,1.21430643318376E-14,
12.5));
#26283=CARTESIAN_POINT('Ctrl Pts',(203.999999999357,-6.80789583155938E-12,
-4.99999999073248));
#26284=CARTESIAN_POINT('Ctrl Pts',(203.999998107003,1.30462817101094,-4.99997309336906));
#26285=CARTESIAN_POINT('Ctrl Pts',(203.985394513333,2.60961113596895,-4.45966517513484));
#26286=CARTESIAN_POINT('Ctrl Pts',(203.96941989844,3.5321022485035,-3.53896223575733));
#26287=CARTESIAN_POINT('Origin',(6.93889390390723E-15,1.21430643318376E-14,
12.5));
#26288=CARTESIAN_POINT('Ctrl Pts',(203.96941989844,3.5321022485035,-3.53896223575733));
#26289=CARTESIAN_POINT('Ctrl Pts',(203.953438052627,4.45501092726816,-2.61784253956751));
#26290=CARTESIAN_POINT('Ctrl Pts',(203.938749239315,4.99865586979689,-1.32397596744565));
#26291=CARTESIAN_POINT('Ctrl Pts',(203.938716348481,4.99999741338323,-0.00508587858850664));
#26292=CARTESIAN_POINT('Origin',(6.93889390390723E-15,1.21430643318376E-14,
12.5));
#26293=CARTESIAN_POINT('Ctrl Pts',(203.938716348481,4.99999741338354,-0.0050858782837947));
#26294=CARTESIAN_POINT('Ctrl Pts',(203.938683457647,5.00133895697019,1.31380421087806));
#26295=CARTESIAN_POINT('Ctrl Pts',(203.953309177856,4.46081412818035,2.60877766178233));
#26296=CARTESIAN_POINT('Ctrl Pts',(203.969311528224,3.5383548016686,3.53271075769143));
#26297=CARTESIAN_POINT('Ctrl Pts',(-203.999999992307,-0.00177162224218141,
-4.99999968613545));
#26298=CARTESIAN_POINT('Ctrl Pts',(-199.974620125014,-0.00177162224218141,
-4.99999968613545));
#26299=CARTESIAN_POINT('Ctrl Pts',(-204.000011327375,1.30344668978611,-5.00046215692299));
#26300=CARTESIAN_POINT('Ctrl Pts',(-199.974631460081,1.30344668978611,-5.00046215692299));
#26301=CARTESIAN_POINT('Ctrl Pts',(-203.985401744253,2.60919356973881,-4.46008193194718));
#26302=CARTESIAN_POINT('Ctrl Pts',(-199.96002187696,2.60919356973881,-4.46008193194718));
#26303=CARTESIAN_POINT('Ctrl Pts',(-203.953438052627,4.45501092726815,-2.61784253956752));
#26304=CARTESIAN_POINT('Ctrl Pts',(-199.928058185333,4.45501092726815,-2.61784253956752));
#26305=CARTESIAN_POINT('Ctrl Pts',(-203.938749239315,4.99865586979689,-1.32397596744566));
#26306=CARTESIAN_POINT('Ctrl Pts',(-199.913369372021,4.99865586979689,-1.32397596744566));
#26307=CARTESIAN_POINT('Ctrl Pts',(-203.938683457647,5.00133895697019,1.31380421087806));
#26308=CARTESIAN_POINT('Ctrl Pts',(-199.913303590353,5.00133895697019,1.31380421087806));
#26309=CARTESIAN_POINT('Ctrl Pts',(-203.953309177856,4.46081412818036,2.60877766178232));
#26310=CARTESIAN_POINT('Ctrl Pts',(-199.927929310562,4.46081412818036,2.60877766178232));
#26311=CARTESIAN_POINT('Ctrl Pts',(-203.985313878591,2.61589547515512,4.45664385360227));
#26312=CARTESIAN_POINT('Ctrl Pts',(-199.959934011298,2.61589547515512,4.45664385360227));
#26313=CARTESIAN_POINT('Ctrl Pts',(-204.,1.32135029102454,5.));
#26314=CARTESIAN_POINT('Ctrl Pts',(-199.974620132706,1.32135029102454,5.));
#26315=CARTESIAN_POINT('Ctrl Pts',(-204.,1.12757025938492E-14,5.));
#26316=CARTESIAN_POINT('Ctrl Pts',(-199.974620132706,1.12757025938492E-14,
5.));
#26317=CARTESIAN_POINT('',(-199.999999992153,-0.00177162224212464,-4.99999968613545));
#26318=CARTESIAN_POINT('',(-203.999999992307,-0.00177162224212464,-4.99999968613545));
#26319=CARTESIAN_POINT('',(-200.,1.12757025938492E-14,5.));
#26320=CARTESIAN_POINT('Ctrl Pts',(-199.999999992153,-0.00177162224212553,
-4.99999968613545));
#26321=CARTESIAN_POINT('Ctrl Pts',(-200.000003044699,0.342832911795084,
-5.00012178795457));
#26322=CARTESIAN_POINT('Ctrl Pts',(-199.999103488806,0.687139768358673,
-4.96254505217617));
#26323=CARTESIAN_POINT('Ctrl Pts',(-199.995649725478,1.36161627231926,-4.81818525737039));
#26324=CARTESIAN_POINT('Ctrl Pts',(-199.993093266738,1.69191513651859,-4.71126381843881));
#26325=CARTESIAN_POINT('Ctrl Pts',(-199.984265249359,2.57114744328878,-4.32586384969142));
#26326=CARTESIAN_POINT('Ctrl Pts',(-199.976588732641,3.09094216142015,-3.97786286150404));
#26327=CARTESIAN_POINT('Ctrl Pts',(-199.964848438847,3.7566290408418,-3.31559837286709));
#26328=CARTESIAN_POINT('Ctrl Pts',(-199.960791072323,3.96423745731536,-3.06259999377541));
#26329=CARTESIAN_POINT('Ctrl Pts',(-199.953200858042,4.33028256236115,-2.51482260163278));
#26330=CARTESIAN_POINT('Ctrl Pts',(-199.94970024374,4.48703860433044,-2.22128115603191));
#26331=CARTESIAN_POINT('Ctrl Pts',(-199.941243543139,4.85350328037375,-1.33869041380516));
#26332=CARTESIAN_POINT('Ctrl Pts',(-199.937819060768,4.98684858575005,-0.719094610949247));
#26333=CARTESIAN_POINT('Ctrl Pts',(-199.937186821031,5.01213494883686,0.572498875379037));
#26334=CARTESIAN_POINT('Ctrl Pts',(-199.940397897686,4.88659419116962,1.19429563481081));
#26335=CARTESIAN_POINT('Ctrl Pts',(-199.950579947465,4.45185250038562,2.36075809964606));
#26336=CARTESIAN_POINT('Ctrl Pts',(-199.9584705221,4.10050445672718,2.93508260604331));
#26337=CARTESIAN_POINT('Ctrl Pts',(-199.96867594025,3.54121851280074,3.53348074247459));
#26338=CARTESIAN_POINT('Ctrl Pts',(-199.970646802731,3.42846001602563,3.64281433950469));
#26339=CARTESIAN_POINT('Ctrl Pts',(-199.980072705603,2.85908134037781,4.1438810712431));
#26340=CARTESIAN_POINT('Ctrl Pts',(-199.987155864494,2.33527138703284,4.45694173085698));
#26341=CARTESIAN_POINT('Ctrl Pts',(-199.997153136931,1.20768836931978,4.88593625759029));
#26342=CARTESIAN_POINT('Ctrl Pts',(-200.,0.605263673202607,5.));
#26343=CARTESIAN_POINT('Ctrl Pts',(-200.,1.13797860024079E-14,5.));
#26344=CARTESIAN_POINT('',(-204.,1.12757025938492E-14,5.));
#26345=CARTESIAN_POINT('Origin',(175.75628980623,72.1784357931688,12.5));
#26346=CARTESIAN_POINT('',(181.394623471171,63.9195500642836,-7.5));
#26347=CARTESIAN_POINT('',(185.006620848663,75.9773008349145,-7.5));
#26348=CARTESIAN_POINT('Origin',(175.75628980623,72.1784357931688,-7.5));
#26349=CARTESIAN_POINT('',(181.394623471171,63.9195500642836,7.5));
#26350=CARTESIAN_POINT('',(181.394623471171,63.9195500642836,7.5));
#26351=CARTESIAN_POINT('',(185.006620848663,75.9773008349145,7.5));
#26352=CARTESIAN_POINT('Origin',(175.75628980623,72.1784357931688,7.5));
#26353=CARTESIAN_POINT('',(185.006620848663,75.9773008349145,12.5));
#26354=CARTESIAN_POINT('Origin',(175.75628980623,-72.1784357931688,7.5));
#26355=CARTESIAN_POINT('',(185.006620848663,-75.9773008349145,-7.5));
#26356=CARTESIAN_POINT('',(181.394623471171,-63.9195500642836,-7.5));
#26357=CARTESIAN_POINT('Origin',(175.75628980623,-72.1784357931688,-7.5));
#26358=CARTESIAN_POINT('',(185.006620848663,-75.9773008349145,7.5));
#26359=CARTESIAN_POINT('',(185.006620848663,-75.9773008349145,12.5));
#26360=CARTESIAN_POINT('',(181.394623471171,-63.9195500642836,7.5));
#26361=CARTESIAN_POINT('Origin',(175.75628980623,-72.1784357931688,7.5));
#26362=CARTESIAN_POINT('',(181.394623471171,-63.9195500642836,7.5));
#26363=CARTESIAN_POINT('Ctrl Pts',(204.,2.16840434497101E-16,5.));
#26364=CARTESIAN_POINT('Ctrl Pts',(199.974623012481,2.16840434497101E-16,
5.));
#26365=CARTESIAN_POINT('Ctrl Pts',(204.,-1.32135029102454,5.));
#26366=CARTESIAN_POINT('Ctrl Pts',(199.974623012481,-1.32135029102454,5.));
#26367=CARTESIAN_POINT('Ctrl Pts',(203.985345962115,-2.61339289425715,4.45784180166547));
#26368=CARTESIAN_POINT('Ctrl Pts',(199.959968974597,-2.61339289425715,4.45784180166547));
#26369=CARTESIAN_POINT('Ctrl Pts',(203.95336383834,-4.45831456152485,2.61258630841649));
#26370=CARTESIAN_POINT('Ctrl Pts',(199.927986850821,-4.45831456152485,2.61258630841649));
#26371=CARTESIAN_POINT('Ctrl Pts',(203.938733312599,-4.99930548519226,1.30702665821117));
#26372=CARTESIAN_POINT('Ctrl Pts',(199.91335632508,-4.99930548519226,1.30702665821117));
#26373=CARTESIAN_POINT('Ctrl Pts',(203.938699292213,-5.00069310016037,-1.30170754686164));
#26374=CARTESIAN_POINT('Ctrl Pts',(199.913322304694,-5.00069310016037,-1.30170754686164));
#26375=CARTESIAN_POINT('Ctrl Pts',(203.953150206634,-4.47024776275284,-2.59986968375128));
#26376=CARTESIAN_POINT('Ctrl Pts',(199.927773219115,-4.47024776275284,-2.59986968375128));
#26377=CARTESIAN_POINT('Ctrl Pts',(203.985508343536,-2.60441550046636,-4.46760084763805));
#26378=CARTESIAN_POINT('Ctrl Pts',(199.960131356017,-2.60441550046636,-4.46760084763805));
#26379=CARTESIAN_POINT('Ctrl Pts',(203.99998865724,-1.3069899342704,-4.99953721534794));
#26380=CARTESIAN_POINT('Ctrl Pts',(199.974611669721,-1.3069899342704,-4.99953721534794));
#26381=CARTESIAN_POINT('Ctrl Pts',(204.000000269508,0.03014770113918,-5.00001099593281));
#26382=CARTESIAN_POINT('Ctrl Pts',(199.974623281989,0.03014770113918,-5.00001099593281));
#26383=CARTESIAN_POINT('Ctrl Pts',(203.999991802598,0.0620673406330946,
-4.99969885211784));
#26384=CARTESIAN_POINT('Ctrl Pts',(199.974614815079,0.0620673406330946,
-4.99969885211784));
#26385=CARTESIAN_POINT('Ctrl Pts',(203.999974785344,0.0939816892981964,
-4.99906559628474));
#26386=CARTESIAN_POINT('Ctrl Pts',(199.974597797825,0.0939816892981964,
-4.99906559628474));
#26387=CARTESIAN_POINT('',(199.999999992153,-0.0017716222421091,-4.99999968613545));
#26388=CARTESIAN_POINT('',(203.999999992307,-0.0017716222421091,-4.99999968613545));
#26389=CARTESIAN_POINT('',(200.,2.16840434497101E-16,5.));
#26390=CARTESIAN_POINT('Ctrl Pts',(200.,2.16840434497101E-16,5.));
#26391=CARTESIAN_POINT('Ctrl Pts',(200.,-0.106689085431466,5.));
#26392=CARTESIAN_POINT('Ctrl Pts',(199.999913765457,-0.212770994842209,
4.99646994038258));
#26393=CARTESIAN_POINT('Ctrl Pts',(199.999745448447,-0.318263257811292,
4.98955065372514));
#26394=CARTESIAN_POINT('Ctrl Pts',(199.999569044592,-0.428823930404872,
4.98229892772));
#26395=CARTESIAN_POINT('Ctrl Pts',(199.999302473722,-0.538737440023033,
4.97132466138716));
#26396=CARTESIAN_POINT('Ctrl Pts',(199.998948825096,-0.64802295579962,4.95672957226209));
#26397=CARTESIAN_POINT('Ctrl Pts',(199.998595176469,-0.757308471576208,
4.94213448313703));
#26398=CARTESIAN_POINT('Ctrl Pts',(199.99815442921,-0.86596652308077,4.92391831426076));
#26399=CARTESIAN_POINT('Ctrl Pts',(199.997628259871,-0.974007405778188,
4.90212506063419));
#26400=CARTESIAN_POINT('Ctrl Pts',(199.99714301239,-1.07364560643664,4.88202673744735));
#26401=CARTESIAN_POINT('Ctrl Pts',(199.996583375234,-1.17308267575688,4.85881220605306));
#26402=CARTESIAN_POINT('Ctrl Pts',(199.995954265594,-1.2719366915673,4.83253690787655));
#26403=CARTESIAN_POINT('Ctrl Pts',(199.995322421172,-1.37122043236585,4.80614738922954));
#26404=CARTESIAN_POINT('Ctrl Pts',(199.994620514446,-1.46991557653475,4.77667056294847));
#26405=CARTESIAN_POINT('Ctrl Pts',(199.993854778568,-1.56764391846616,4.74421450831223));
#26406=CARTESIAN_POINT('Ctrl Pts',(199.993085898829,-1.66577350100801,4.71162519973023));
#26407=CARTESIAN_POINT('Ctrl Pts',(199.99225268186,-1.7629278505394,4.67603232253121));
#26408=CARTESIAN_POINT('Ctrl Pts',(199.991362450625,-1.85873994433746,4.6375952416386));
#26409=CARTESIAN_POINT('Ctrl Pts',(199.991194313089,-1.87683592740531,4.63033564906069));
#26410=CARTESIAN_POINT('Ctrl Pts',(199.991024144215,-1.89488408714042,4.62297473700675));
#26411=CARTESIAN_POINT('Ctrl Pts',(199.990851996581,-1.9128820355165,4.61551376963032));
#26412=CARTESIAN_POINT('Ctrl Pts',(199.989904874678,-2.0119031527102,4.57446501732134));
#26413=CARTESIAN_POINT('Ctrl Pts',(199.988899457036,-2.10927871151272,4.5304446155066));
#26414=CARTESIAN_POINT('Ctrl Pts',(199.987843468119,-2.20502888607493,4.48349555287741));
#26415=CARTESIAN_POINT('Ctrl Pts',(199.986757493131,-2.30349800157137,4.43521331536066));
#26416=CARTESIAN_POINT('Ctrl Pts',(199.985618017166,-2.40024873740821,4.38383369997872));
#26417=CARTESIAN_POINT('Ctrl Pts',(199.984432539852,-2.49528004230067,4.32935098461817));
#26418=CARTESIAN_POINT('Ctrl Pts',(199.983247062538,-2.59031134719313,4.27486826925761));
#26419=CARTESIAN_POINT('Ctrl Pts',(199.982015562515,-2.68362377963686,4.21728220600999));
#26420=CARTESIAN_POINT('Ctrl Pts',(199.980744946283,-2.7751848100423,4.15653780080854));
#26421=CARTESIAN_POINT('Ctrl Pts',(199.979687255077,-2.85140239185876,4.1059727115688));
#26422=CARTESIAN_POINT('Ctrl Pts',(199.97860051674,-2.92654667296149,4.05311678026368));
#26423=CARTESIAN_POINT('Ctrl Pts',(199.977494181696,-3.00027821604381,3.99812698249647));
#26424=CARTESIAN_POINT('Ctrl Pts',(199.976393937544,-3.07360383248166,3.94343992929629));
#26425=CARTESIAN_POINT('Ctrl Pts',(199.975274327858,-3.14553183008494,3.88664264849037));
#26426=CARTESIAN_POINT('Ctrl Pts',(199.974145117418,-3.21575710331105,3.82793200561578));
#26427=CARTESIAN_POINT('Ctrl Pts',(199.973025477997,-3.28538715766477,3.76971898533551));
#26428=CARTESIAN_POINT('Ctrl Pts',(199.971896415521,-3.35334289802745,3.70962515179665));
#26429=CARTESIAN_POINT('Ctrl Pts',(199.970767675607,-3.4193606338094,3.64788081938912));
#26430=CARTESIAN_POINT('Ctrl Pts',(199.970092075891,-3.45887510736828,3.61092416279631));
#26431=CARTESIAN_POINT('Ctrl Pts',(199.969416594983,-3.49769595480584,3.57337692877078));
#26432=CARTESIAN_POINT('Ctrl Pts',(199.968743327175,-3.53577320405375,3.53529459154323));
#26433=CARTESIAN_POINT('Ctrl Pts',(199.968742852571,-3.53580004566718,3.53526774634316));
#26434=CARTESIAN_POINT('Ctrl Pts',(199.968742377966,-3.53582688694626,3.53524090084241));
#26435=CARTESIAN_POINT('Ctrl Pts',(199.96874190336,-3.535853727891,3.53521405504098));
#26436=CARTESIAN_POINT('Ctrl Pts',(199.967444306764,-3.60923812432215,3.46181638020426));
#26437=CARTESIAN_POINT('Ctrl Pts',(199.96615206232,-3.68005108078868,3.38615882914448));
#26438=CARTESIAN_POINT('Ctrl Pts',(199.96487158156,-3.74836710179276,3.30830569203447));
#26439=CARTESIAN_POINT('Ctrl Pts',(199.963578976184,-3.81732999356935,3.22971537910238));
#26440=CARTESIAN_POINT('Ctrl Pts',(199.962298340419,-3.88374870865775,3.14888724771301));
#26441=CARTESIAN_POINT('Ctrl Pts',(199.961036490357,-3.94766064633092,3.06585149887276));
#26442=CARTESIAN_POINT('Ctrl Pts',(199.959767630887,-4.01192760623837,2.98235449759437));
#26443=CARTESIAN_POINT('Ctrl Pts',(199.958517747431,-4.07366014492571,2.8966247993813));
#26444=CARTESIAN_POINT('Ctrl Pts',(199.957294270602,-4.13285266907493,2.80866409496906));
#26445=CARTESIAN_POINT('Ctrl Pts',(199.95715658911,-4.1395137801211,2.79876561491249));
#26446=CARTESIAN_POINT('Ctrl Pts',(199.95701924272,-4.14614267734788,2.78883885657405));
#26447=CARTESIAN_POINT('Ctrl Pts',(199.956882242583,-4.15273931588746,2.77888380377105));
#26448=CARTESIAN_POINT('Ctrl Pts',(199.955449809748,-4.22171181380409,2.67479672144946));
#26449=CARTESIAN_POINT('Ctrl Pts',(199.954061738709,-4.28685552062367,2.56806446766188));
#26450=CARTESIAN_POINT('Ctrl Pts',(199.952733419607,-4.34795058538834,2.45918048333498));
#26451=CARTESIAN_POINT('Ctrl Pts',(199.951403408826,-4.40912345767029,2.35015782999244));
#26452=CARTESIAN_POINT('Ctrl Pts',(199.950133324122,-4.46623711429618,2.23897860351396));
#26453=CARTESIAN_POINT('Ctrl Pts',(199.9489378304,-4.51911833478099,2.12615944454101));
#26454=CARTESIAN_POINT('Ctrl Pts',(199.948189148404,-4.55223537839354,2.05550606374186));
#26455=CARTESIAN_POINT('Ctrl Pts',(199.947469703677,-4.58369344773626,1.98420990101436));
#26456=CARTESIAN_POINT('Ctrl Pts',(199.946782884472,-4.61346010600003,1.91240038834254));
#26457=CARTESIAN_POINT('Ctrl Pts',(199.945244027409,-4.68015397830596,1.75150713569573));
#26458=CARTESIAN_POINT('Ctrl Pts',(199.943856293168,-4.73891591400558,1.58668724722363));
#26459=CARTESIAN_POINT('Ctrl Pts',(199.942652291709,-4.78917781231223,1.41890179219067));
#26460=CARTESIAN_POINT('Ctrl Pts',(199.941603883869,-4.83294434421902,1.27279932255469));
#26461=CARTESIAN_POINT('Ctrl Pts',(199.940694808887,-4.87026604656124,1.12444934574699));
#26462=CARTESIAN_POINT('Ctrl Pts',(199.93994672643,-4.90078596068217,0.97451290256118));
#26463=CARTESIAN_POINT('Ctrl Pts',(199.939427256788,-4.92197903732505,0.870396799239052));
#26464=CARTESIAN_POINT('Ctrl Pts',(199.938988357527,-4.93977769850371,0.766104978382168));
#26465=CARTESIAN_POINT('Ctrl Pts',(199.938631378381,-4.95419932372897,0.661646608836728));
#26466=CARTESIAN_POINT('Ctrl Pts',(199.938257638965,-4.96929804824499,0.552283889966628));
#26467=CARTESIAN_POINT('Ctrl Pts',(199.937973662438,-4.98069584574989,0.442738086255646));
#26468=CARTESIAN_POINT('Ctrl Pts',(199.937782272973,-4.98835300268517,0.333005356104372));
#26469=CARTESIAN_POINT('Ctrl Pts',(199.937602385329,-4.99554999187858,0.229867170517087));
#26470=CARTESIAN_POINT('Ctrl Pts',(199.937504286432,-4.9994420905526,0.126563270571131));
#26471=CARTESIAN_POINT('Ctrl Pts',(199.93749163394,-4.99994428099095,0.0230865138943863));
#26472=CARTESIAN_POINT('Ctrl Pts',(199.937490824953,-4.999976390507,0.0164703214593889));
#26473=CARTESIAN_POINT('Ctrl Pts',(199.937490365772,-4.99999462369657,0.00985342259099019));
#26474=CARTESIAN_POINT('Ctrl Pts',(199.937490257555,-4.99999895100585,0.00323581564284581));
#26475=CARTESIAN_POINT('Ctrl Pts',(199.937490254414,-4.99999907661166,0.00304373094603564));
#26476=CARTESIAN_POINT('Ctrl Pts',(199.937490251566,-4.99999919050222,0.00285164428893937));
#26477=CARTESIAN_POINT('Ctrl Pts',(199.937490249012,-4.99999929267631,0.00265955567476706));
#26478=CARTESIAN_POINT('Ctrl Pts',(199.937489018394,-5.00004851957456,-0.0898876539113899));
#26479=CARTESIAN_POINT('Ctrl Pts',(199.937555311217,-4.99741975626774,-0.182864304129975));
#26480=CARTESIAN_POINT('Ctrl Pts',(199.937688351935,-4.99210548145091,-0.275917349116757));
#26481=CARTESIAN_POINT('Ctrl Pts',(199.937822179922,-4.98675975940393,-0.369521035653615));
#26482=CARTESIAN_POINT('Ctrl Pts',(199.938023535793,-4.97869670329359,-0.463201602984161));
#26483=CARTESIAN_POINT('Ctrl Pts',(199.938290146696,-4.96796164010122,-0.556598752708217));
#26484=CARTESIAN_POINT('Ctrl Pts',(199.938559009805,-4.95713589206307,-0.650784878330061));
#26485=CARTESIAN_POINT('Ctrl Pts',(199.938894221282,-4.94359288463427,-0.744682328172369));
#26486=CARTESIAN_POINT('Ctrl Pts',(199.939292143069,-4.92743182557626,-0.837927234917629));
#26487=CARTESIAN_POINT('Ctrl Pts',(199.939485856061,-4.9195644325493,-0.883319948754859));
#26488=CARTESIAN_POINT('Ctrl Pts',(199.939694412193,-4.91107738214136,-0.928558146494761));
#26489=CARTESIAN_POINT('Ctrl Pts',(199.939917296751,-4.90198647168346,-0.97360081736077));
#26490=CARTESIAN_POINT('Ctrl Pts',(199.940432998254,-4.88095228143802,-1.07781877358698));
#26491=CARTESIAN_POINT('Ctrl Pts',(199.941025461062,-4.85667571130338,-1.18106633062347));
#26492=CARTESIAN_POINT('Ctrl Pts',(199.941688795583,-4.82922287471879,-1.28335964226709));
#26493=CARTESIAN_POINT('Ctrl Pts',(199.942377799029,-4.80070770109351,-1.3896113781573));
#26494=CARTESIAN_POINT('Ctrl Pts',(199.943143277803,-4.76876581556843,-1.49483421604507));
#26495=CARTESIAN_POINT('Ctrl Pts',(199.943979937156,-4.73341334147567,-1.59903492791101));
#26496=CARTESIAN_POINT('Ctrl Pts',(199.944816596509,-4.6980608673829,-1.70323563977696));
#26497=CARTESIAN_POINT('Ctrl Pts',(199.945724457359,-4.65929760501924,-1.80641482603871));
#26498=CARTESIAN_POINT('Ctrl Pts',(199.946699239106,-4.6170838617614,-1.908558894064));
#26499=CARTESIAN_POINT('Ctrl Pts',(199.947580381323,-4.57892525707422,-2.00089079386994));
#26500=CARTESIAN_POINT('Ctrl Pts',(199.948516093717,-4.53794998813828,-2.09234828060927));
#26501=CARTESIAN_POINT('Ctrl Pts',(199.949497749981,-4.49428712854347,-2.18256058459083));
#26502=CARTESIAN_POINT('Ctrl Pts',(199.950476582438,-4.45074986841002,-2.27251338617393));
#26503=CARTESIAN_POINT('Ctrl Pts',(199.951501077809,-4.40454064733321,-2.36122769950356));
#26504=CARTESIAN_POINT('Ctrl Pts',(199.952561949357,-4.35583435975879,-2.44835766561793));
#26505=CARTESIAN_POINT('Ctrl Pts',(199.953616658299,-4.30741100717498,-2.53498149346203));
#26506=CARTESIAN_POINT('Ctrl Pts',(199.954707305024,-4.25651975128412,-2.6200389191733));
#26507=CARTESIAN_POINT('Ctrl Pts',(199.955824291131,-4.20337569014082,-2.7032180367477));
#26508=CARTESIAN_POINT('Ctrl Pts',(199.956150084129,-4.18787508284152,-2.72747901359602));
#26509=CARTESIAN_POINT('Ctrl Pts',(199.956478115705,-4.17218309328504,-2.75158040235868));
#26510=CARTESIAN_POINT('Ctrl Pts',(199.956808143247,-4.15630571119065,-2.77551499023631));
#26511=CARTESIAN_POINT('Ctrl Pts',(199.958041623657,-4.09696387664856,-2.86497069176347));
#26512=CARTESIAN_POINT('Ctrl Pts',(199.959307171522,-4.03482709407707,-2.95241426289202));
#26513=CARTESIAN_POINT('Ctrl Pts',(199.96059705484,-3.96986498972616,-3.03782589478993));
#26514=CARTESIAN_POINT('Ctrl Pts',(199.961908169114,-3.90383363549083,-3.12464336749992));
#26515=CARTESIAN_POINT('Ctrl Pts',(199.963244443955,-3.83488312168669,-3.2093620691675));
#26516=CARTESIAN_POINT('Ctrl Pts',(199.964598170151,-3.76293631072323,-3.29192868462007));
#26517=CARTESIAN_POINT('Ctrl Pts',(199.965951896348,-3.69098949975976,-3.37449530007264));
#26518=CARTESIAN_POINT('Ctrl Pts',(199.967323092874,-3.6160462267238,-3.45491039126157));
#26519=CARTESIAN_POINT('Ctrl Pts',(199.968704181971,-3.5379864023958,-3.5330797025401));
#26520=CARTESIAN_POINT('Ctrl Pts',(199.968708043156,-3.53776816634513,-3.53329824468933));
#26521=CARTESIAN_POINT('Ctrl Pts',(199.968711904499,-3.53754990941597,-3.53351676574182));
#26522=CARTESIAN_POINT('Ctrl Pts',(199.968715766001,-3.5373316316096,-3.53373526569467));
#26523=CARTESIAN_POINT('Ctrl Pts',(199.970460080863,-3.43873133816247,-3.63243590699128));
#26524=CARTESIAN_POINT('Ctrl Pts',(199.972198401154,-3.3362985501167,-3.7264135444678));
#26525=CARTESIAN_POINT('Ctrl Pts',(199.97390904525,-3.23039259847156,-3.81566238109671));
#26526=CARTESIAN_POINT('Ctrl Pts',(199.97565820908,-3.12210189066793,-3.9069208943253));
#26527=CARTESIAN_POINT('Ctrl Pts',(199.977378458043,-3.0101793631941,-3.993235586349));
#26528=CARTESIAN_POINT('Ctrl Pts',(199.979046584675,-2.89497000257252,-4.07456267017766));
#26529=CARTESIAN_POINT('Ctrl Pts',(199.979597895658,-2.85689364512564,-4.10144103402992));
#26530=CARTESIAN_POINT('Ctrl Pts',(199.980143511741,-2.81845799249297,-4.12777428808935));
#26531=CARTESIAN_POINT('Ctrl Pts',(199.980682588089,-2.779674729519,-4.15355987795212));
#26532=CARTESIAN_POINT('Ctrl Pts',(199.98193608989,-2.68949290247773,-4.21351851543761));
#26533=CARTESIAN_POINT('Ctrl Pts',(199.983159605131,-2.59702475383697,-4.27078090386246));
#26534=CARTESIAN_POINT('Ctrl Pts',(199.984340873962,-2.5026016568129,-4.32510605962663));
#26535=CARTESIAN_POINT('Ctrl Pts',(199.985531674906,-2.40741662352963,-4.37986958595127));
#26536=CARTESIAN_POINT('Ctrl Pts',(199.986679526008,-2.31024539867246,-4.43164800699807));
#26537=CARTESIAN_POINT('Ctrl Pts',(199.987772232853,-2.21145908473947,-4.48023721650249));
#26538=CARTESIAN_POINT('Ctrl Pts',(199.988854707941,-2.11359777432304,-4.52837145215608));
#26539=CARTESIAN_POINT('Ctrl Pts',(199.989883049636,-2.01415200784204,-4.57337579928167));
#26540=CARTESIAN_POINT('Ctrl Pts',(199.990846026127,-1.91350614164553,-4.61509643176659));
#26541=CARTESIAN_POINT('Ctrl Pts',(199.991792578593,-1.81457683876425,-4.65610549893921));
#26542=CARTESIAN_POINT('Ctrl Pts',(199.992673774464,-1.71473372931631,-4.69384912859574));
#26543=CARTESIAN_POINT('Ctrl Pts',(199.993486393832,-1.61399492664038,-4.72837579232869));
#26544=CARTESIAN_POINT('Ctrl Pts',(199.994324637516,-1.51007952850957,-4.76399118493446));
#26545=CARTESIAN_POINT('Ctrl Pts',(199.995089935849,-1.40521060202274,-4.79618398138844));
#26546=CARTESIAN_POINT('Ctrl Pts',(199.995777839267,-1.29938616025944,-4.82495380140898));
#26547=CARTESIAN_POINT('Ctrl Pts',(199.996465742685,-1.19356171849615,-4.85372362142952));
#26548=CARTESIAN_POINT('Ctrl Pts',(199.997076272279,-1.08678118101417,-4.87907068709132));
#26549=CARTESIAN_POINT('Ctrl Pts',(199.997603740834,-0.979029072207799,
-4.90093718328589));
#26550=CARTESIAN_POINT('Ctrl Pts',(199.998041002663,-0.889704535897929,
-4.91906411049815));
#26551=CARTESIAN_POINT('Ctrl Pts',(199.998421910603,-0.79950470998423,-4.93483341824134));
#26552=CARTESIAN_POINT('Ctrl Pts',(199.998743013132,-0.708780352003267,
-4.94811276998379));
#26553=CARTESIAN_POINT('Ctrl Pts',(199.999062276332,-0.618575678342215,
-4.96131605537501));
#26554=CARTESIAN_POINT('Ctrl Pts',(199.999322402601,-0.527852889977945,
-4.97205769316921));
#26555=CARTESIAN_POINT('Ctrl Pts',(199.999521129845,-0.436966717445114,
-4.98025786975492));
#26556=CARTESIAN_POINT('Ctrl Pts',(199.99971810453,-0.346882062393027,-4.98838572967578));
#26557=CARTESIAN_POINT('Ctrl Pts',(199.999854746094,-0.256637304781016,
-4.99401669744085));
#26558=CARTESIAN_POINT('Ctrl Pts',(199.999930165345,-0.166581446645463,
-4.9971239797482));
#26559=CARTESIAN_POINT('Ctrl Pts',(199.99997625447,-0.11154780929047,-4.99902285730267));
#26560=CARTESIAN_POINT('Ctrl Pts',(199.999999506613,-0.0565847596115855,
-4.99998026449957));
#26561=CARTESIAN_POINT('Ctrl Pts',(199.999999992153,-0.00177162224210914,
-4.99999968613545));
#26562=CARTESIAN_POINT('',(204.,2.16840434497101E-16,5.));
#26563=CARTESIAN_POINT('Origin',(-198.037532067764,0.,-7.5));
#26564=CARTESIAN_POINT('',(-198.037532067764,-27.9488084273619,-7.5));
#26565=CARTESIAN_POINT('',(-198.037532067764,27.948808427362,-7.5));
#26566=CARTESIAN_POINT('Origin',(-198.037532067764,0.,-7.5));
#26567=CARTESIAN_POINT('',(-198.037532067764,-27.948808427362,7.5));
#26568=CARTESIAN_POINT('',(-198.037532067764,-27.9488084273619,-7.5));
#26569=CARTESIAN_POINT('',(-198.037532067764,27.9488084273619,7.5));
#26570=CARTESIAN_POINT('Origin',(-198.037532067764,0.,7.5));
#26571=CARTESIAN_POINT('',(-198.037532067764,27.9488084273619,-7.5));
#26572=CARTESIAN_POINT('Origin',(0.,0.,-78.2106781186548));
#26573=CARTESIAN_POINT('',(2.47860448411075,17.2857000454522,-7.50000000000001));
#26574=CARTESIAN_POINT('',(-2.0402937480676,17.3428979029341,-7.50000000000001));
#26575=CARTESIAN_POINT('Origin',(0.,0.,-7.50000000000001));
#26576=CARTESIAN_POINT('',(-2.0402937480676,17.3428979029341,15.));
#26577=CARTESIAN_POINT('',(-2.0402937480676,17.3428979029341,-78.2106781186548));
#26578=CARTESIAN_POINT('',(2.47860448411075,17.2857000454522,15.));
#26579=CARTESIAN_POINT('Origin',(0.,0.,15.));
#26580=CARTESIAN_POINT('',(2.47860448411075,17.2857000454522,-78.2106781186548));
#26581=CARTESIAN_POINT('Origin',(0.745999527119512,1.21430643318376E-14,
-78.2106781186548));
#26582=CARTESIAN_POINT('',(23.3816321893336,-10.6126402926561,7.5));
#26583=CARTESIAN_POINT('',(25.6668951325528,1.98719959316974,7.5));
#26584=CARTESIAN_POINT('Origin',(0.745999527119512,1.21430643318376E-14,
7.5));
#26585=CARTESIAN_POINT('',(25.6668951325528,1.98719959316974,15.));
#26586=CARTESIAN_POINT('',(25.6668951325528,1.98719959316974,-78.2106781186548));
#26587=CARTESIAN_POINT('',(23.3816321893336,-10.6126402926561,15.));
#26588=CARTESIAN_POINT('Origin',(0.745999527119512,1.21430643318376E-14,
15.));
#26589=CARTESIAN_POINT('',(23.3816321893336,-10.6126402926561,-78.2106781186548));
#26590=CARTESIAN_POINT('Origin',(6.93889390390723E-15,1.21430643318376E-14,
12.5));
#26591=CARTESIAN_POINT('',(204.,-1.28397303707684E-14,-12.5));
#26592=CARTESIAN_POINT('Origin',(6.93889390390723E-15,1.21430643318376E-14,
-12.5));
#26593=CARTESIAN_POINT('',(204.,-1.28397303707684E-14,12.5));
#26594=CARTESIAN_POINT('',(204.,-1.28397303707684E-14,12.5));
#26595=CARTESIAN_POINT('',(204.,-1.28397303707684E-14,12.5));
#26596=CARTESIAN_POINT('Origin',(6.93889390390723E-15,1.21430643318376E-14,
12.5));
#26597=CARTESIAN_POINT('Origin',(6.93889390390723E-15,1.21430643318376E-14,
12.5));
#26598=CARTESIAN_POINT('',(200.,-1.23498716511094E-14,12.5));
#26599=CARTESIAN_POINT('Origin',(6.93889390390723E-15,1.21430643318376E-14,
12.5));
#26600=CARTESIAN_POINT('',(200.,-1.23498716511094E-14,12.5));
#26601=CARTESIAN_POINT('',(200.,-1.22464679914735E-14,-4.99999998173599));
#26602=CARTESIAN_POINT('Ctrl Pts',(200.,-1.40355392239111E-14,-4.99999998173599));
#26603=CARTESIAN_POINT('Ctrl Pts',(200.,-0.00059053984960231,-4.99999999390701));
#26604=CARTESIAN_POINT('Ctrl Pts',(199.999999997384,-0.00118108060876073,
-4.99999989537881));
#26605=CARTESIAN_POINT('Ctrl Pts',(199.999999992153,-0.00177162224210903,
-4.99999968613545));
#26606=CARTESIAN_POINT('',(200.,-1.23498716511094E-14,-12.5));
#26607=CARTESIAN_POINT('',(200.,-1.23498716511094E-14,12.5));
#26608=CARTESIAN_POINT('Origin',(6.93889390390723E-15,1.21430643318376E-14,
-12.5));
#26609=CARTESIAN_POINT('Ctrl Pts',(200.,4.16333634234434E-16,5.));
#26610=CARTESIAN_POINT('Ctrl Pts',(200.,0.605263673276849,5.));
#26611=CARTESIAN_POINT('Ctrl Pts',(199.997153136931,1.20768836943757,4.88593625756298));
#26612=CARTESIAN_POINT('Ctrl Pts',(199.98715586449,2.33527138738033,4.45694173064992));
#26613=CARTESIAN_POINT('Ctrl Pts',(199.980072705597,2.85908134082911,4.14388107086821));
#26614=CARTESIAN_POINT('Ctrl Pts',(199.970646802724,3.42846001642483,3.64281433909067));
#26615=CARTESIAN_POINT('Ctrl Pts',(199.968675940244,3.54121851313504,3.53348074213681));
#26616=CARTESIAN_POINT('Ctrl Pts',(199.958470522096,4.10050445692498,2.93508260589754));
#26617=CARTESIAN_POINT('Ctrl Pts',(199.950579947462,4.45185250050671,2.36075809949633));
#26618=CARTESIAN_POINT('Ctrl Pts',(199.940397897687,4.886594191151,1.19429563484653));
#26619=CARTESIAN_POINT('Ctrl Pts',(199.937186821031,5.01213494884488,0.572498875413951));
#26620=CARTESIAN_POINT('Ctrl Pts',(199.937819060768,4.98684858574211,-0.719094611003917));
#26621=CARTESIAN_POINT('Ctrl Pts',(199.94124354314,4.85350328035862,-1.33869041386019));
#26622=CARTESIAN_POINT('Ctrl Pts',(199.949700243741,4.48703860430459,-2.22128115608432));
#26623=CARTESIAN_POINT('Ctrl Pts',(199.953200858042,4.33028256233193,-2.51482260168344));
#26624=CARTESIAN_POINT('Ctrl Pts',(199.960791072323,3.96423745728102,-3.06259999381995));
#26625=CARTESIAN_POINT('Ctrl Pts',(199.964848438847,3.75662904080501,-3.31559837290915));
#26626=CARTESIAN_POINT('Ctrl Pts',(199.976588732642,3.09094216137304,-3.97786286154054));
#26627=CARTESIAN_POINT('Ctrl Pts',(199.98426524936,2.57114744323512,-4.32586384972337));
#26628=CARTESIAN_POINT('Ctrl Pts',(199.993093266739,1.69191513646751,-4.71126381845647));
#26629=CARTESIAN_POINT('Ctrl Pts',(199.995649725478,1.36161627227762,-4.81818525738156));
#26630=CARTESIAN_POINT('Ctrl Pts',(199.999100531766,0.687717241141568,-4.96242145431402));
#26631=CARTESIAN_POINT('Ctrl Pts',(200.,0.344012953281906,-4.99999289163375));
#26632=CARTESIAN_POINT('Ctrl Pts',(200.,-1.42247325030098E-14,-4.99999998173599));
#26633=CARTESIAN_POINT('Ctrl Pts',(-200.,1.12757025938492E-14,5.));
#26634=CARTESIAN_POINT('Ctrl Pts',(-200.,-0.106689084767584,5.));
#26635=CARTESIAN_POINT('Ctrl Pts',(-199.999913765458,-0.212770993513047,
4.99646994042657));
#26636=CARTESIAN_POINT('Ctrl Pts',(-199.99974544845,-0.318263255820032,
4.98955065385575));
#26637=CARTESIAN_POINT('Ctrl Pts',(-199.999569044596,-0.42882392875795,
4.98229892787329));
#26638=CARTESIAN_POINT('Ctrl Pts',(-199.999302473726,-0.538737438711796,
4.97132466154013));
#26639=CARTESIAN_POINT('Ctrl Pts',(-199.998948825099,-0.648022954821224,
4.95672957239276));
#26640=CARTESIAN_POINT('Ctrl Pts',(-199.998595176472,-0.757308470930653,
4.94213448324538));
#26641=CARTESIAN_POINT('Ctrl Pts',(-199.998154429211,-0.865966522765234,
4.9239183143248));
#26642=CARTESIAN_POINT('Ctrl Pts',(-199.997628259871,-0.97400740579531,
4.90212506063074));
#26643=CARTESIAN_POINT('Ctrl Pts',(-199.997143012391,-1.07364560623553,
4.88202673748756));
#26644=CARTESIAN_POINT('Ctrl Pts',(-199.996583375236,-1.17308267533976,
4.85881220615028));
#26645=CARTESIAN_POINT('Ctrl Pts',(-199.995954265598,-1.27193669093702,
4.83253690804408));
#26646=CARTESIAN_POINT('Ctrl Pts',(-199.995322421178,-1.37122043151843,
4.8061473894685));
#26647=CARTESIAN_POINT('Ctrl Pts',(-199.994620514454,-1.46991557547311,
4.77667056327245));
#26648=CARTESIAN_POINT('Ctrl Pts',(-199.993854778578,-1.56764391719393,
4.74421450873475));
#26649=CARTESIAN_POINT('Ctrl Pts',(-199.993085898841,-1.66577349952316,
4.71162520025208));
#26650=CARTESIAN_POINT('Ctrl Pts',(-199.992252681875,-1.76292784884562,
4.67603232316609));
#26651=CARTESIAN_POINT('Ctrl Pts',(-199.991362450643,-1.8587399424392,4.63759524240013));
#26652=CARTESIAN_POINT('Ctrl Pts',(-199.991194313101,-1.87683592615673,
4.63033564957001));
#26653=CARTESIAN_POINT('Ctrl Pts',(-199.991024144221,-1.89488408653804,
4.62297473725664));
#26654=CARTESIAN_POINT('Ctrl Pts',(-199.99085199658,-1.91288203555658,4.61551376961371));
#26655=CARTESIAN_POINT('Ctrl Pts',(-199.989904874678,-2.01190315274628,
4.57446501730539));
#26656=CARTESIAN_POINT('Ctrl Pts',(-199.988899457035,-2.10927871154764,
4.53044461549043));
#26657=CARTESIAN_POINT('Ctrl Pts',(-199.987843468119,-2.20502888611135,
4.48349555285956));
#26658=CARTESIAN_POINT('Ctrl Pts',(-199.986757493131,-2.30349800160627,
4.43521331534257));
#26659=CARTESIAN_POINT('Ctrl Pts',(-199.985618017165,-2.40024873744451,
4.38383369995907));
#26660=CARTESIAN_POINT('Ctrl Pts',(-199.984432539851,-2.49528004234097,
4.32935098459506));
#26661=CARTESIAN_POINT('Ctrl Pts',(-199.983247062538,-2.59031134723743,
4.27486826923105));
#26662=CARTESIAN_POINT('Ctrl Pts',(-199.982015562515,-2.68362377968778,
4.21728220597808));
#26663=CARTESIAN_POINT('Ctrl Pts',(-199.980744946282,-2.77518481010207,
4.15653780076889));
#26664=CARTESIAN_POINT('Ctrl Pts',(-199.979687255074,-2.85140239203149,
4.10597271145264));
#26665=CARTESIAN_POINT('Ctrl Pts',(-199.978600516736,-2.9265466732396,4.05311678006709));
#26666=CARTESIAN_POINT('Ctrl Pts',(-199.97749418169,-3.00027821641985,3.99812698221601));
#26667=CARTESIAN_POINT('Ctrl Pts',(-199.976393937536,-3.07360383295553,
3.94343992893212));
#26668=CARTESIAN_POINT('Ctrl Pts',(-199.975274327849,-3.14553183064925,
3.88664264803906));
#26669=CARTESIAN_POINT('Ctrl Pts',(-199.974145117408,-3.21575710395861,
3.8279320050744));
#26670=CARTESIAN_POINT('Ctrl Pts',(-199.973025477985,-3.28538715839498,
3.76971898470472));
#26671=CARTESIAN_POINT('Ctrl Pts',(-199.971896415508,-3.35334289883324,
3.70962515107354));
#26672=CARTESIAN_POINT('Ctrl Pts',(-199.970767675592,-3.41936063468391,
3.64788081857121));
#26673=CARTESIAN_POINT('Ctrl Pts',(-199.970092075881,-3.45887510795394,
3.61092416223028));
#26674=CARTESIAN_POINT('Ctrl Pts',(-199.969416594978,-3.49769595511179,
3.57337692846561));
#26675=CARTESIAN_POINT('Ctrl Pts',(-199.968743327174,-3.53577320409041,
3.53529459150656));
#26676=CARTESIAN_POINT('Ctrl Pts',(-199.968742852571,-3.53580004569161,
3.53526774631872));
#26677=CARTESIAN_POINT('Ctrl Pts',(-199.968742377966,-3.53582688695847,
3.53524090083019));
#26678=CARTESIAN_POINT('Ctrl Pts',(-199.96874190336,-3.53585372789099,3.53521405504099));
#26679=CARTESIAN_POINT('Ctrl Pts',(-199.967444306764,-3.60923812433126,
3.46181638019514));
#26680=CARTESIAN_POINT('Ctrl Pts',(-199.96615206232,-3.68005108080915,3.3861588291228));
#26681=CARTESIAN_POINT('Ctrl Pts',(-199.96487158156,-3.7483671018263,3.30830569199624));
#26682=CARTESIAN_POINT('Ctrl Pts',(-199.963578976183,-3.8173299936106,3.22971537905371));
#26683=CARTESIAN_POINT('Ctrl Pts',(-199.962298340418,-3.88374870870884,
3.14888724765019));
#26684=CARTESIAN_POINT('Ctrl Pts',(-199.961036490355,-3.94766064639338,
3.06585149879162));
#26685=CARTESIAN_POINT('Ctrl Pts',(-199.959767630885,-4.01192760630376,
2.98235449750583));
#26686=CARTESIAN_POINT('Ctrl Pts',(-199.95851774743,-4.07366014499625,2.8966247992817));
#26687=CARTESIAN_POINT('Ctrl Pts',(-199.9572942706,-4.13285266915211,2.80866409485437));
#26688=CARTESIAN_POINT('Ctrl Pts',(-199.957156589108,-4.13951378018764,
2.79876561481302));
#26689=CARTESIAN_POINT('Ctrl Pts',(-199.957019242719,-4.14614267740391,
2.78883885648985));
#26690=CARTESIAN_POINT('Ctrl Pts',(-199.956882242582,-4.1527393159331,2.77888380370217));
#26691=CARTESIAN_POINT('Ctrl Pts',(-199.95544980972,-4.22171181515478,2.6747967194074));
#26692=CARTESIAN_POINT('Ctrl Pts',(-199.954061738656,-4.28685552312269,
2.56806446356432));
#26693=CARTESIAN_POINT('Ctrl Pts',(-199.952733419531,-4.34795058887662,
2.45918047711815));
#26694=CARTESIAN_POINT('Ctrl Pts',(-199.951403408728,-4.40912346210568,
2.350157821731));
#26695=CARTESIAN_POINT('Ctrl Pts',(-199.950133324005,-4.46623711952495,
2.23897859314705));
#26696=CARTESIAN_POINT('Ctrl Pts',(-199.948937830268,-4.51911834064776,
2.12615943202458));
#26697=CARTESIAN_POINT('Ctrl Pts',(-199.948189148319,-4.55223538211244,
2.05550605531406));
#26698=CARTESIAN_POINT('Ctrl Pts',(-199.947469703636,-4.58369344950168,
1.98420989675678));
#26699=CARTESIAN_POINT('Ctrl Pts',(-199.946782884472,-4.61346010601319,
1.91240038831081));
#26700=CARTESIAN_POINT('Ctrl Pts',(-199.945244027512,-4.6801539738286,1.75150714649393));
#26701=CARTESIAN_POINT('Ctrl Pts',(-199.943856293354,-4.7389159061174,1.58668726934914));
#26702=CARTESIAN_POINT('Ctrl Pts',(-199.942652291952,-4.78917780218821,
1.41890182598691));
#26703=CARTESIAN_POINT('Ctrl Pts',(-199.941603884009,-4.83294433847652,
1.27279934538775));
#26704=CARTESIAN_POINT('Ctrl Pts',(-199.940694808944,-4.87026604422707,
1.12444935722674));
#26705=CARTESIAN_POINT('Ctrl Pts',(-199.939946726429,-4.90078596069864,
0.974512902480285));
#26706=CARTESIAN_POINT('Ctrl Pts',(-199.939427256788,-4.92197903733681,
0.870396799172517));
#26707=CARTESIAN_POINT('Ctrl Pts',(-199.938988357527,-4.93977769851255,
0.766104978326001));
#26708=CARTESIAN_POINT('Ctrl Pts',(-199.938631378381,-4.95419932373587,
0.661646608786745));
#26709=CARTESIAN_POINT('Ctrl Pts',(-199.938257638965,-4.96929804824874,
0.552283889931227));
#26710=CARTESIAN_POINT('Ctrl Pts',(-199.937973662438,-4.98069584575212,
0.442738086230268));
#26711=CARTESIAN_POINT('Ctrl Pts',(-199.937782272973,-4.98835300268657,
0.333005356084353));
#26712=CARTESIAN_POINT('Ctrl Pts',(-199.937602385329,-4.99554999187818,
0.229867170516646));
#26713=CARTESIAN_POINT('Ctrl Pts',(-199.937504286432,-4.99944209055195,
0.126563270586194));
#26714=CARTESIAN_POINT('Ctrl Pts',(-199.93749163394,-4.99994428099082,0.023086513920902));
#26715=CARTESIAN_POINT('Ctrl Pts',(-199.937490824953,-4.99997639050698,
0.0164703214711166));
#26716=CARTESIAN_POINT('Ctrl Pts',(-199.937490365772,-4.9999946236966,0.00985342258791087));
#26717=CARTESIAN_POINT('Ctrl Pts',(-199.937490257555,-4.99999895100586,
0.0032358156249388));
#26718=CARTESIAN_POINT('Ctrl Pts',(-199.937490254414,-4.99999907661167,
0.00304373093410148));
#26719=CARTESIAN_POINT('Ctrl Pts',(-199.937490251566,-4.99999919050223,
0.00285164428297918));
#26720=CARTESIAN_POINT('Ctrl Pts',(-199.937490249012,-4.99999929267631,
0.00265955567477993));
#26721=CARTESIAN_POINT('Ctrl Pts',(-199.937489018394,-5.00004851957442,
-0.0898876536395686));
#26722=CARTESIAN_POINT('Ctrl Pts',(-199.937555311217,-4.99741975628316,
-0.182864303586234));
#26723=CARTESIAN_POINT('Ctrl Pts',(-199.937688351934,-4.99210548149748,
-0.275917348301421));
#26724=CARTESIAN_POINT('Ctrl Pts',(-199.93782217992,-4.98675975948198,-0.369521034562259));
#26725=CARTESIAN_POINT('Ctrl Pts',(-199.93802353579,-4.97869670341907,-0.463201601617108));
#26726=CARTESIAN_POINT('Ctrl Pts',(-199.938290146692,-4.96796164028995,
-0.55659875106629));
#26727=CARTESIAN_POINT('Ctrl Pts',(-199.938559009798,-4.95713589231543,
-0.650784876412101));
#26728=CARTESIAN_POINT('Ctrl Pts',(-199.938894221274,-4.94359288496629,
-0.744682325979206));
#26729=CARTESIAN_POINT('Ctrl Pts',(-199.939292143059,-4.92743182600384,
-0.83792723245062));
#26730=CARTESIAN_POINT('Ctrl Pts',(-199.939485856053,-4.91956443285371,
-0.883319947133576));
#26731=CARTESIAN_POINT('Ctrl Pts',(-199.939694412189,-4.91107738229964,
-0.92855814571286));
#26732=CARTESIAN_POINT('Ctrl Pts',(-199.939917296751,-4.90198647167366,
-0.973600817409316));
#26733=CARTESIAN_POINT('Ctrl Pts',(-199.940432998255,-4.88095228142656,
-1.07781877363846));
#26734=CARTESIAN_POINT('Ctrl Pts',(-199.941025461063,-4.8566757112893,-1.18106633068164));
#26735=CARTESIAN_POINT('Ctrl Pts',(-199.941688795583,-4.82922287470041,
-1.28335964233559));
#26736=CARTESIAN_POINT('Ctrl Pts',(-199.94237779903,-4.80070770107679,-1.38961137821365));
#26737=CARTESIAN_POINT('Ctrl Pts',(-199.943143277804,-4.76876581555304,
-1.49483421609362));
#26738=CARTESIAN_POINT('Ctrl Pts',(-199.943979937156,-4.73341334146045,
-1.59903492795587));
#26739=CARTESIAN_POINT('Ctrl Pts',(-199.944816596509,-4.69806086736786,
-1.70323563981812));
#26740=CARTESIAN_POINT('Ctrl Pts',(-199.94572445736,-4.65929760500322,-1.80641482608029));
#26741=CARTESIAN_POINT('Ctrl Pts',(-199.946699239106,-4.6170838617425,-1.90855889410973));
#26742=CARTESIAN_POINT('Ctrl Pts',(-199.947580381328,-4.57892525687886,
-2.00089079434012));
#26743=CARTESIAN_POINT('Ctrl Pts',(-199.948516093726,-4.53794998774401,
-2.09234828148755));
#26744=CARTESIAN_POINT('Ctrl Pts',(-199.949497749995,-4.49428712792918,
-2.18256058586003));
#26745=CARTESIAN_POINT('Ctrl Pts',(-199.950476582457,-4.45074986757737,
-2.27251338783079));
#26746=CARTESIAN_POINT('Ctrl Pts',(-199.951501077833,-4.40454064626135,
-2.36122770153106));
#26747=CARTESIAN_POINT('Ctrl Pts',(-199.952561949386,-4.35583435842811,
-2.44835766799837));
#26748=CARTESIAN_POINT('Ctrl Pts',(-199.953616658333,-4.30741100559012,
-2.53498149618775));
#26749=CARTESIAN_POINT('Ctrl Pts',(-199.954707305064,-4.25651974942602,
-2.62003892222701));
#26750=CARTESIAN_POINT('Ctrl Pts',(-199.955824291176,-4.20337568799156,
-2.70321804011165));
#26751=CARTESIAN_POINT('Ctrl Pts',(-199.956150084159,-4.18787508138827,
-2.72747901582816));
#26752=CARTESIAN_POINT('Ctrl Pts',(-199.95647811572,-4.17218309254555,-2.7515804034736));
#26753=CARTESIAN_POINT('Ctrl Pts',(-199.956808143247,-4.15630571118181,
-2.77551499024965));
#26754=CARTESIAN_POINT('Ctrl Pts',(-199.958041623657,-4.09696387666182,
-2.86497069174285));
#26755=CARTESIAN_POINT('Ctrl Pts',(-199.959307171522,-4.03482709411232,
-2.95241426284234));
#26756=CARTESIAN_POINT('Ctrl Pts',(-199.960597054839,-3.96986498978254,
-3.03782589471581));
#26757=CARTESIAN_POINT('Ctrl Pts',(-199.961908169113,-3.90383363553538,
-3.12464336744474));
#26758=CARTESIAN_POINT('Ctrl Pts',(-199.963244443954,-3.83488312171559,
-3.2093620691339));
#26759=CARTESIAN_POINT('Ctrl Pts',(-199.964598170151,-3.76293631073179,
-3.29192868461025));
#26760=CARTESIAN_POINT('Ctrl Pts',(-199.965951896348,-3.69098949974798,
-3.3744953000866));
#26761=CARTESIAN_POINT('Ctrl Pts',(-199.967323092875,-3.61604622668702,
-3.4549103913015));
#26762=CARTESIAN_POINT('Ctrl Pts',(-199.968704181972,-3.53798640232844,
-3.53307970260756));
#26763=CARTESIAN_POINT('Ctrl Pts',(-199.968708043157,-3.53776816630022,
-3.5332982447343));
#26764=CARTESIAN_POINT('Ctrl Pts',(-199.9687119045,-3.53754990939351,-3.5335167657643));
#26765=CARTESIAN_POINT('Ctrl Pts',(-199.968715766001,-3.53733163160961,
-3.53373526569466));
#26766=CARTESIAN_POINT('Ctrl Pts',(-199.970460080778,-3.43873134294032,
-3.63243590220857));
#26767=CARTESIAN_POINT('Ctrl Pts',(-199.972198400985,-3.33629856007218,
-3.72641353533234));
#26768=CARTESIAN_POINT('Ctrl Pts',(-199.973909045,-3.23039261393604,-3.81566236806452));
#26769=CARTESIAN_POINT('Ctrl Pts',(-199.975658208745,-3.12210191187783,
-3.90692087721395));
#26770=CARTESIAN_POINT('Ctrl Pts',(-199.977378457628,-3.01017939050342,
-3.99323556564552));
#26771=CARTESIAN_POINT('Ctrl Pts',(-199.979046584187,-2.89497003626135,
-4.07456264639649));
#26772=CARTESIAN_POINT('Ctrl Pts',(-199.979597895336,-2.85689366779627,
-4.10144101849774));
#26773=CARTESIAN_POINT('Ctrl Pts',(-199.980143511582,-2.81845800392829,
-4.12777428048652));
#26774=CARTESIAN_POINT('Ctrl Pts',(-199.980682588089,-2.77967472951125,
-4.15355987795727));
#26775=CARTESIAN_POINT('Ctrl Pts',(-199.981936089878,-2.68949290329997,
-4.21351851489069));
#26776=CARTESIAN_POINT('Ctrl Pts',(-199.983159605109,-2.59702475552414,
-4.27078090281776));
#26777=CARTESIAN_POINT('Ctrl Pts',(-199.98434087393,-2.50260165939654,-4.32510605814017));
#26778=CARTESIAN_POINT('Ctrl Pts',(-199.985531674863,-2.40741662703508,
-4.37986958400906));
#26779=CARTESIAN_POINT('Ctrl Pts',(-199.986679525956,-2.31024540313252,
-4.43164800465818));
#26780=CARTESIAN_POINT('Ctrl Pts',(-199.987772232793,-2.2114590901831,-4.48023721382498));
#26781=CARTESIAN_POINT('Ctrl Pts',(-199.988854707903,-2.11359777799008,
-4.52837145049721));
#26782=CARTESIAN_POINT('Ctrl Pts',(-199.989883049618,-2.01415200967174,
-4.57337579852419));
#26783=CARTESIAN_POINT('Ctrl Pts',(-199.990846026127,-1.91350614160602,
-4.61509643178297));
#26784=CARTESIAN_POINT('Ctrl Pts',(-199.991792578594,-1.81457683872722,
-4.65610549895359));
#26785=CARTESIAN_POINT('Ctrl Pts',(-199.992673774464,-1.71473372927819,
-4.69384912860981));
#26786=CARTESIAN_POINT('Ctrl Pts',(-199.993486393832,-1.61399492659733,
-4.72837579234345));
#26787=CARTESIAN_POINT('Ctrl Pts',(-199.994324637517,-1.51007952847902,
-4.7639911849439));
#26788=CARTESIAN_POINT('Ctrl Pts',(-199.99508993585,-1.40521060200091,-4.79618398139478));
#26789=CARTESIAN_POINT('Ctrl Pts',(-199.995777839267,-1.29938616024233,
-4.82495380141363));
#26790=CARTESIAN_POINT('Ctrl Pts',(-199.996465742685,-1.19356171848376,
-4.85372362143249));
#26791=CARTESIAN_POINT('Ctrl Pts',(-199.997076272279,-1.08678118100251,
-4.87907068709403));
#26792=CARTESIAN_POINT('Ctrl Pts',(-199.997603740834,-0.979029072192739,
-4.90093718328894));
#26793=CARTESIAN_POINT('Ctrl Pts',(-199.998041002663,-0.889704535842363,
-4.91906411050914));
#26794=CARTESIAN_POINT('Ctrl Pts',(-199.998421910603,-0.799504709890456,
-4.93483341825751));
#26795=CARTESIAN_POINT('Ctrl Pts',(-199.998743013132,-0.708780351873667,
-4.94811277000276));
#26796=CARTESIAN_POINT('Ctrl Pts',(-199.999062276332,-0.618575678176499,
-4.96131605539684));
#26797=CARTESIAN_POINT('Ctrl Pts',(-199.999322402602,-0.527852889778465,
-4.97205769319153));
#26798=CARTESIAN_POINT('Ctrl Pts',(-199.999521129845,-0.436966717214281,
-4.98025786977575));
#26799=CARTESIAN_POINT('Ctrl Pts',(-199.999718104531,-0.346882062129988,
-4.98838572969523));
#26800=CARTESIAN_POINT('Ctrl Pts',(-199.999854746094,-0.256637304488128,
-4.99401669745692));
#26801=CARTESIAN_POINT('Ctrl Pts',(-199.999930165345,-0.166581446325115,
-4.99712397975926));
#26802=CARTESIAN_POINT('Ctrl Pts',(-199.99997625447,-0.111547809076515,
-4.99902285730641));
#26803=CARTESIAN_POINT('Ctrl Pts',(-199.999999506613,-0.056584759504595,
-4.99998026449961));
#26804=CARTESIAN_POINT('Ctrl Pts',(-199.999999992153,-0.00177162224212468,
-4.99999968613545));
#26805=CARTESIAN_POINT('',(198.037532067764,27.948808427362,-7.5));
#26806=CARTESIAN_POINT('Origin',(6.93889390390723E-15,1.21430643318376E-14,
-7.5));
#26807=CARTESIAN_POINT('',(198.037532067764,27.948808427362,7.5));
#26808=CARTESIAN_POINT('Origin',(6.93889390390723E-15,1.21430643318376E-14,
7.5));
#26809=CARTESIAN_POINT('',(198.037532067764,27.948808427362,-7.5));
#26810=CARTESIAN_POINT('',(-185.006620848663,75.9773008349145,7.5));
#26811=CARTESIAN_POINT('',(-185.006620848663,75.9773008349145,-7.5));
#26812=CARTESIAN_POINT('',(-185.006620848663,75.9773008349145,12.5));
#26813=CARTESIAN_POINT('Origin',(6.93889390390723E-15,1.21430643318376E-14,
-7.5));
#26814=CARTESIAN_POINT('Origin',(6.93889390390723E-15,1.21430643318376E-14,
7.5));
#26815=CARTESIAN_POINT('',(-185.006620848663,-75.9773008349146,-7.5));
#26816=CARTESIAN_POINT('Origin',(6.93889390390723E-15,1.21430643318376E-14,
-7.5));
#26817=CARTESIAN_POINT('',(-185.006620848663,-75.9773008349146,7.5));
#26818=CARTESIAN_POINT('',(-185.006620848663,-75.9773008349146,12.5));
#26819=CARTESIAN_POINT('Origin',(6.93889390390723E-15,1.21430643318376E-14,
7.5));
#26820=CARTESIAN_POINT('',(198.037532067764,-27.948808427362,-7.5));
#26821=CARTESIAN_POINT('Origin',(6.93889390390723E-15,1.21430643318376E-14,
-7.5));
#26822=CARTESIAN_POINT('',(198.037532067764,-27.9488084273619,7.5));
#26823=CARTESIAN_POINT('',(198.037532067764,-27.9488084273619,-7.5));
#26824=CARTESIAN_POINT('Origin',(6.93889390390723E-15,1.21430643318376E-14,
7.5));
#26825=CARTESIAN_POINT('Origin',(0.,0.,7.5));
#26826=CARTESIAN_POINT('',(-181.394623471171,-63.9195500642836,7.5));
#26827=CARTESIAN_POINT('Origin',(-175.75628980623,-72.1784357931688,7.5));
#26828=CARTESIAN_POINT('',(-43.7076833558927,-63.9537123387768,7.5));
#26829=CARTESIAN_POINT('Origin',(-112.576160096458,-164.723060254401,7.5));
#26830=CARTESIAN_POINT('',(43.7076833558926,-63.9537123387769,7.5));
#26831=CARTESIAN_POINT('Origin',(0.,0.,7.5));
#26832=CARTESIAN_POINT('Origin',(112.576160096458,-164.723060254401,7.5));
#26833=CARTESIAN_POINT('Origin',(198.037532067764,4.85052059515657E-14,
7.5));
#26834=CARTESIAN_POINT('',(43.7076833558927,63.9537123387769,7.5));
#26835=CARTESIAN_POINT('Origin',(112.576160096458,164.723060254401,7.5));
#26836=CARTESIAN_POINT('',(-43.7076833558927,63.9537123387769,7.5));
#26837=CARTESIAN_POINT('Origin',(0.,0.,7.5));
#26838=CARTESIAN_POINT('',(-181.394623471171,63.9195500642836,7.5));
#26839=CARTESIAN_POINT('Origin',(-112.576160096458,164.723060254401,7.5));
#26840=CARTESIAN_POINT('Origin',(-175.75628980623,72.1784357931688,7.5));
#26841=CARTESIAN_POINT('',(49.8000928868158,55.4601300422384,7.5));
#26842=CARTESIAN_POINT('',(45.9698706712208,58.6740680906711,7.5));
#26843=CARTESIAN_POINT('',(49.8000928868158,55.4601300422384,7.5));
#26844=CARTESIAN_POINT('',(18.2451455071118,17.854408138354,7.5));
#26845=CARTESIAN_POINT('',(49.8000928868158,55.4601300422384,7.5));
#26846=CARTESIAN_POINT('',(24.7730106681704,6.90671670389171,7.5));
#26847=CARTESIAN_POINT('Origin',(0.745999527119512,1.21430643318376E-14,
7.5));
#26848=CARTESIAN_POINT('',(72.9299279571745,15.3980805296896,7.5));
#26849=CARTESIAN_POINT('',(72.9299279571745,15.3980805296896,7.5));
#26850=CARTESIAN_POINT('',(73.7981688455092,10.4740417646285,7.5));
#26851=CARTESIAN_POINT('',(73.7981688455092,10.4740417646286,7.5));
#26852=CARTESIAN_POINT('',(73.7981688455092,10.4740417646286,7.5));
#26853=CARTESIAN_POINT('',(65.7652614261009,-35.0828400417365,7.5));
#26854=CARTESIAN_POINT('',(65.7652614261009,-35.0828400417365,7.5));
#26855=CARTESIAN_POINT('',(63.265261426101,-39.4129670606588,7.5));
#26856=CARTESIAN_POINT('',(63.2652614261009,-39.4129670606588,7.5));
#26857=CARTESIAN_POINT('',(20.8166938897999,-14.9052751668619,7.5));
#26858=CARTESIAN_POINT('',(63.2652614261009,-39.4129670606588,7.5));
#26859=CARTESIAN_POINT('',(10.9648337349804,-22.8161220945246,7.5));
#26860=CARTESIAN_POINT('Origin',(0.745999527119512,1.21430643318376E-14,
7.5));
#26861=CARTESIAN_POINT('',(27.8282981742883,-69.1481098552981,7.5));
#26862=CARTESIAN_POINT('',(27.8282981742883,-69.1481098552981,7.5));
#26863=CARTESIAN_POINT('',(23.1298350703588,-70.8582105719264,7.5));
#26864=CARTESIAN_POINT('',(23.1298350703588,-70.8582105719264,7.5));
#26865=CARTESIAN_POINT('',(6.21815778991956,-24.393759118817,7.5));
#26866=CARTESIAN_POINT('',(23.1298350703588,-70.8582105719264,7.5));
#26867=CARTESIAN_POINT('',(-6.09183989625028,-24.0467035582886,7.5));
#26868=CARTESIAN_POINT('Origin',(0.745999527119512,1.21430643318376E-14,
7.5));
#26869=CARTESIAN_POINT('',(-23.1298350703578,-70.8582105719268,7.5));
#26870=CARTESIAN_POINT('',(-23.1298350703578,-70.8582105719268,7.5));
#26871=CARTESIAN_POINT('',(-27.8282981742874,-69.1481098552985,7.5));
#26872=CARTESIAN_POINT('',(-27.8282981742874,-69.1481098552985,7.5));
#26873=CARTESIAN_POINT('',(-10.7420901590486,-22.2041391493244,7.5));
#26874=CARTESIAN_POINT('',(-27.8282981742874,-69.1481098552985,7.5));
#26875=CARTESIAN_POINT('',(-19.7626328986541,-14.296712769882,7.5));
#26876=CARTESIAN_POINT('Origin',(0.745999527119512,1.21430643318376E-14,
7.5));
#26877=CARTESIAN_POINT('',(-63.2652614261004,-39.4129670606597,7.5));
#26878=CARTESIAN_POINT('',(-63.2652614261004,-39.4129670606597,7.5));
#26879=CARTESIAN_POINT('',(-65.7652614261004,-35.0828400417375,7.5));
#26880=CARTESIAN_POINT('',(-65.7652614261004,-35.0828400417375,7.5));
#26881=CARTESIAN_POINT('',(-22.2199439289764,-9.94193926282494,7.5));
#26882=CARTESIAN_POINT('',(-65.7652614261004,-35.0828400417375,7.5));
#26883=CARTESIAN_POINT('',(-22.1041836607387,-10.1424419289105,7.5));
#26884=CARTESIAN_POINT('',(-22.2199439289764,-9.94193926282494,7.5));
#26885=CARTESIAN_POINT('',(-24.1016880072274,2.75543539126987,7.50000000000001));
#26886=CARTESIAN_POINT('Origin',(0.745999527119512,1.21430643318376E-14,
7.5));
#26887=CARTESIAN_POINT('',(-24.2802608359423,1.74269855430126,7.5));
#26888=CARTESIAN_POINT('',(-23.4120199476077,6.6667373193623,7.5));
#26889=CARTESIAN_POINT('',(-73.7981688455094,10.4740417646276,7.5));
#26890=CARTESIAN_POINT('',(-73.7981688455094,10.4740417646276,7.5));
#26891=CARTESIAN_POINT('',(-72.9299279571747,15.3980805296886,7.5));
#26892=CARTESIAN_POINT('',(-72.9299279571747,15.3980805296886,7.5));
#26893=CARTESIAN_POINT('',(-23.4120199476077,6.6667373193623,7.5));
#26894=CARTESIAN_POINT('',(-72.9299279571747,15.3980805296886,7.5));
#26895=CARTESIAN_POINT('',(-23.545603499947,5.90914734758,7.50000000000001));
#26896=CARTESIAN_POINT('',(-23.4120199476077,6.6667373193623,7.5));
#26897=CARTESIAN_POINT('',(-17.5548310250611,17.0317233743498,7.5));
#26898=CARTESIAN_POINT('Origin',(0.745999527119512,1.21430643318376E-14,
7.5));
#26899=CARTESIAN_POINT('',(-49.8000928868165,55.4601300422377,7.5));
#26900=CARTESIAN_POINT('',(-49.8000928868165,55.4601300422377,7.5));
#26901=CARTESIAN_POINT('',(-45.9698706712216,58.6740680906704,7.5));
#26902=CARTESIAN_POINT('',(-45.9698706712216,58.6740680906704,7.5));
#26903=CARTESIAN_POINT('',(-13.7984652228223,20.3336800687357,7.5));
#26904=CARTESIAN_POINT('',(-45.9698706712216,58.6740680906704,7.5));
#26905=CARTESIAN_POINT('',(-2.5,24.7883740303785,7.5));
#26906=CARTESIAN_POINT('Origin',(0.745999527119512,1.21430643318376E-14,
7.5));
#26907=CARTESIAN_POINT('',(-2.5,74.4958071023965,7.5));
#26908=CARTESIAN_POINT('',(-2.5,74.4958071023965,7.5));
#26909=CARTESIAN_POINT('',(2.5,74.4958071023965,7.5));
#26910=CARTESIAN_POINT('',(2.5,74.4958071023965,7.5));
#26911=CARTESIAN_POINT('',(2.5,24.9383937401978,7.5));
#26912=CARTESIAN_POINT('',(2.5,74.4958071023965,7.5));
#26913=CARTESIAN_POINT('',(14.3410668781608,20.9803275408334,7.5));
#26914=CARTESIAN_POINT('Origin',(0.745999527119512,1.21430643318376E-14,
7.5));
#26915=CARTESIAN_POINT('',(45.9698706712208,58.6740680906711,7.5));
#26916=CARTESIAN_POINT('Origin',(0.745999527119512,1.21430643318376E-14,
-78.2106781186548));
#26917=CARTESIAN_POINT('',(18.2451455071118,17.854408138354,15.));
#26918=CARTESIAN_POINT('',(18.2451455071118,17.854408138354,-78.2106781186548));
#26919=CARTESIAN_POINT('',(24.7730106681704,6.90671670389171,15.));
#26920=CARTESIAN_POINT('Origin',(0.745999527119512,1.21430643318376E-14,
15.));
#26921=CARTESIAN_POINT('',(24.7730106681704,6.90671670389171,-78.2106781186548));
#26922=CARTESIAN_POINT('Origin',(0.745999527119512,1.21430643318376E-14,
-78.2106781186548));
#26923=CARTESIAN_POINT('',(20.8166938897999,-14.9052751668619,15.));
#26924=CARTESIAN_POINT('',(20.8166938897999,-14.9052751668619,-78.2106781186548));
#26925=CARTESIAN_POINT('',(10.9648337349804,-22.8161220945246,15.));
#26926=CARTESIAN_POINT('Origin',(0.745999527119512,1.21430643318376E-14,
15.));
#26927=CARTESIAN_POINT('',(10.9648337349804,-22.8161220945246,-78.2106781186548));
#26928=CARTESIAN_POINT('Origin',(0.745999527119512,1.21430643318376E-14,
-78.2106781186548));
#26929=CARTESIAN_POINT('',(6.21815778991956,-24.393759118817,15.));
#26930=CARTESIAN_POINT('',(6.21815778991956,-24.393759118817,-78.2106781186548));
#26931=CARTESIAN_POINT('',(-6.09183989625028,-24.0467035582886,15.));
#26932=CARTESIAN_POINT('Origin',(0.745999527119512,1.21430643318376E-14,
15.));
#26933=CARTESIAN_POINT('',(-6.09183989625028,-24.0467035582886,-78.2106781186548));
#26934=CARTESIAN_POINT('Origin',(0.745999527119512,1.21430643318376E-14,
-78.2106781186548));
#26935=CARTESIAN_POINT('',(-10.7420901590486,-22.2041391493244,15.));
#26936=CARTESIAN_POINT('',(-10.7420901590486,-22.2041391493244,-78.2106781186548));
#26937=CARTESIAN_POINT('',(-19.7626328986541,-14.296712769882,15.));
#26938=CARTESIAN_POINT('Origin',(0.745999527119512,1.21430643318376E-14,
15.));
#26939=CARTESIAN_POINT('',(-19.7626328986541,-14.296712769882,-78.2106781186548));
#26940=CARTESIAN_POINT('Origin',(0.745999527119512,1.21430643318376E-14,
-78.2106781186548));
#26941=CARTESIAN_POINT('',(-22.1041836607387,-10.1424419289105,15.));
#26942=CARTESIAN_POINT('',(-22.1041836607387,-10.1424419289104,-78.2106781186548));
#26943=CARTESIAN_POINT('',(-24.1016880072274,2.75543539126994,15.));
#26944=CARTESIAN_POINT('Origin',(0.745999527119512,1.21430643318376E-14,
15.));
#26945=CARTESIAN_POINT('',(-24.1016880072274,2.75543539126993,-78.2106781186548));
#26946=CARTESIAN_POINT('Origin',(0.745999527119512,1.21430643318376E-14,
-78.2106781186548));
#26947=CARTESIAN_POINT('',(14.3410668781608,20.9803275408334,15.));
#26948=CARTESIAN_POINT('',(14.3410668781608,20.9803275408334,-78.2106781186548));
#26949=CARTESIAN_POINT('',(2.5,24.9383937401978,15.));
#26950=CARTESIAN_POINT('',(2.5,24.9383937401978,-78.2106781186548));
#26951=CARTESIAN_POINT('Origin',(0.745999527119512,1.21430643318376E-14,
15.));
#26952=CARTESIAN_POINT('Origin',(0.745999527119512,1.21430643318376E-14,
-78.2106781186548));
#26953=CARTESIAN_POINT('',(-23.545603499947,5.90914734757994,15.));
#26954=CARTESIAN_POINT('',(-23.545603499947,5.90914734757994,-78.2106781186548));
#26955=CARTESIAN_POINT('',(-17.5548310250611,17.0317233743498,15.));
#26956=CARTESIAN_POINT('Origin',(0.745999527119512,1.21430643318376E-14,
15.));
#26957=CARTESIAN_POINT('',(-17.5548310250611,17.0317233743498,-78.2106781186548));
#26958=CARTESIAN_POINT('Origin',(0.745999527119512,1.21430643318376E-14,
-78.2106781186548));
#26959=CARTESIAN_POINT('',(-13.7984652228223,20.3336800687357,15.));
#26960=CARTESIAN_POINT('',(-13.7984652228223,20.3336800687357,-78.2106781186548));
#26961=CARTESIAN_POINT('',(-2.5,24.7883740303784,15.));
#26962=CARTESIAN_POINT('Origin',(0.745999527119512,1.21430643318376E-14,
15.));
#26963=CARTESIAN_POINT('',(-2.5,24.7883740303784,-78.2106781186548));
#26964=CARTESIAN_POINT('Origin',(0.,0.,12.5));
#26965=CARTESIAN_POINT('Origin',(0.,0.,-12.5));
#26966=CARTESIAN_POINT('Origin',(-112.576160096458,-164.723060254401,7.5));
#26967=CARTESIAN_POINT('',(-181.394623471171,-63.9195500642836,-7.5));
#26968=CARTESIAN_POINT('',(-181.394623471171,-63.9195500642835,7.5));
#26969=CARTESIAN_POINT('',(-43.7076833558927,-63.9537123387768,-7.5));
#26970=CARTESIAN_POINT('Origin',(-112.576160096458,-164.723060254401,-7.5));
#26971=CARTESIAN_POINT('',(-43.7076833558927,-63.9537123387768,7.5));
#26972=CARTESIAN_POINT('Origin',(0.,0.,7.5));
#26973=CARTESIAN_POINT('',(43.7076833558926,-63.9537123387769,-7.5));
#26974=CARTESIAN_POINT('Origin',(0.,0.,-7.5));
#26975=CARTESIAN_POINT('',(43.7076833558926,-63.9537123387769,7.5));
#26976=CARTESIAN_POINT('Origin',(112.576160096458,-164.723060254401,7.5));
#26977=CARTESIAN_POINT('Origin',(112.576160096458,-164.723060254401,-7.5));
#26978=CARTESIAN_POINT('Origin',(112.576160096458,164.723060254401,7.5));
#26979=CARTESIAN_POINT('',(43.7076833558927,63.9537123387769,-7.5));
#26980=CARTESIAN_POINT('Origin',(112.576160096458,164.723060254401,-7.5));
#26981=CARTESIAN_POINT('',(43.7076833558927,63.9537123387769,7.5));
#26982=CARTESIAN_POINT('Origin',(0.,0.,7.5));
#26983=CARTESIAN_POINT('',(-43.7076833558927,63.9537123387769,-7.5));
#26984=CARTESIAN_POINT('Origin',(0.,0.,-7.5));
#26985=CARTESIAN_POINT('',(-43.7076833558927,63.9537123387769,7.5));
#26986=CARTESIAN_POINT('Origin',(-112.576160096458,164.723060254401,7.5));
#26987=CARTESIAN_POINT('',(-181.394623471171,63.9195500642836,-7.5));
#26988=CARTESIAN_POINT('Origin',(-112.576160096458,164.723060254401,-7.5));
#26989=CARTESIAN_POINT('',(-181.394623471171,63.9195500642836,7.5));
#26990=CARTESIAN_POINT('Origin',(0.,0.,-7.5));
#26991=CARTESIAN_POINT('Origin',(-175.75628980623,72.1784357931688,-7.5));
#26992=CARTESIAN_POINT('Origin',(198.037532067764,4.85052059515657E-14,
-7.5));
#26993=CARTESIAN_POINT('Origin',(-175.75628980623,-72.1784357931688,-7.5));
#26994=CARTESIAN_POINT('',(2.47860448411075,21.6999127067652,-7.5));
#26995=CARTESIAN_POINT('',(2.47860448411075,0.,-7.5));
#26996=CARTESIAN_POINT('',(-2.0402937480676,21.6999127067652,-7.5));
#26997=CARTESIAN_POINT('',(0.,21.6999127067652,-7.5));
#26998=CARTESIAN_POINT('',(-2.0402937480676,0.,-7.5));
#26999=CARTESIAN_POINT('Origin',(0.,0.,15.));
#27000=CARTESIAN_POINT('',(18.4844395432205,18.139587665573,15.));
#27001=CARTESIAN_POINT('',(17.4795738527292,16.9420353688553,15.));
#27002=CARTESIAN_POINT('',(14.6542173276256,21.3535257140057,15.));
#27003=CARTESIAN_POINT('',(18.4844395432205,18.139587665573,15.));
#27004=CARTESIAN_POINT('',(13.6493516371343,20.1559734172879,15.));
#27005=CARTESIAN_POINT('',(2.5,25.7772990420638,15.));
#27006=CARTESIAN_POINT('',(2.5,24.2140055445719,15.));
#27007=CARTESIAN_POINT('',(-2.5,25.7772990420638,15.));
#27008=CARTESIAN_POINT('',(2.5,25.7772990420638,15.));
#27009=CARTESIAN_POINT('',(-2.5,24.2140055445719,15.));
#27010=CARTESIAN_POINT('',(-14.6542173276259,21.3535257140055,15.));
#27011=CARTESIAN_POINT('',(-13.6493516371345,20.1559734172877,15.));
#27012=CARTESIAN_POINT('',(-18.4844395432208,18.1395876655728,15.));
#27013=CARTESIAN_POINT('',(-14.6542173276259,21.3535257140055,15.));
#27014=CARTESIAN_POINT('',(-17.4795738527294,16.942035368855,15.));
#27015=CARTESIAN_POINT('',(-23.4120199476077,6.6667373193623,15.));
#27016=CARTESIAN_POINT('',(-23.4120199476077,6.6667373193623,15.));
#27017=CARTESIAN_POINT('',(-24.9515635041713,6.93820038636033,15.));
#27018=CARTESIAN_POINT('',(-23.4120199476077,6.6667373193623,15.));
#27019=CARTESIAN_POINT('',(-25.8198043925059,2.01416162129929,15.));
#27020=CARTESIAN_POINT('',(-24.9515635041713,6.93820038636033,15.));
#27021=CARTESIAN_POINT('',(-24.2802608359423,1.74269855430126,15.));
#27022=CARTESIAN_POINT('',(-24.2802608359423,1.74269855430126,15.));
#27023=CARTESIAN_POINT('',(-23.4120199476077,6.6667373193623,15.));
#27024=CARTESIAN_POINT('',(-22.2199439289764,-9.94193926282494,15.));
#27025=CARTESIAN_POINT('',(-22.2199439289764,-9.94193926282494,15.));
#27026=CARTESIAN_POINT('',(-23.5737958113755,-10.7235860115709,15.));
#27027=CARTESIAN_POINT('',(-22.2199439289764,-9.94193926282494,15.));
#27028=CARTESIAN_POINT('',(-21.0737958113755,-15.0537130304931,15.));
#27029=CARTESIAN_POINT('',(-23.5737958113755,-10.7235860115709,15.));
#27030=CARTESIAN_POINT('',(-19.7199439289764,-14.2720662817471,15.));
#27031=CARTESIAN_POINT('',(-11.1655870648799,-23.3676873353049,15.));
#27032=CARTESIAN_POINT('',(-10.6309091988076,-21.8986719715891,15.));
#27033=CARTESIAN_POINT('',(-6.46712396095037,-25.0777880519332,15.));
#27034=CARTESIAN_POINT('',(-11.1655870648799,-23.3676873353049,15.));
#27035=CARTESIAN_POINT('',(-5.93244609487809,-23.6087726882175,15.));
#27036=CARTESIAN_POINT('',(6.4671239609507,-25.0777880519331,15.));
#27037=CARTESIAN_POINT('',(5.93244609487841,-23.6087726882174,15.));
#27038=CARTESIAN_POINT('',(11.1655870648802,-23.3676873353048,15.));
#27039=CARTESIAN_POINT('',(6.4671239609507,-25.0777880519331,15.));
#27040=CARTESIAN_POINT('',(10.6309091988079,-21.898671971589,15.));
#27041=CARTESIAN_POINT('',(21.0737958113757,-15.0537130304928,15.));
#27042=CARTESIAN_POINT('',(19.7199439289766,-14.2720662817468,15.));
#27043=CARTESIAN_POINT('',(23.5737958113756,-10.7235860115706,15.));
#27044=CARTESIAN_POINT('',(21.0737958113757,-15.0537130304928,15.));
#27045=CARTESIAN_POINT('',(22.2199439289766,-9.94193926282463,15.));
#27046=CARTESIAN_POINT('',(25.8198043925059,2.01416162129963,15.));
#27047=CARTESIAN_POINT('',(24.2802608359423,1.74269855430158,15.));
#27048=CARTESIAN_POINT('',(24.9515635041712,6.93820038636067,15.));
#27049=CARTESIAN_POINT('',(25.8198043925059,2.01416162129963,15.));
#27050=CARTESIAN_POINT('',(23.4120199476076,6.66673731936261,15.));
#27051=CARTESIAN_POINT('',(2.47860448411075,21.6999127067652,15.));
#27052=CARTESIAN_POINT('',(2.47860448411075,0.,15.));
#27053=CARTESIAN_POINT('',(-2.0402937480676,21.6999127067652,15.));
#27054=CARTESIAN_POINT('',(-2.0402937480676,0.,15.));
#27055=CARTESIAN_POINT('',(0.,21.6999127067652,15.));
#27056=CARTESIAN_POINT('Origin',(198.037532067764,4.85052059515657E-14,
-7.5));
#27057=CARTESIAN_POINT('Origin',(2.5,25.7772990420638,15.));
#27058=CARTESIAN_POINT('',(-2.5,25.7772990420638,15.));
#27059=CARTESIAN_POINT('',(2.5,25.7772990420638,15.));
#27060=CARTESIAN_POINT('Origin',(2.5,0.,0.));
#27061=CARTESIAN_POINT('Origin',(-2.5,0.,0.));
#27062=CARTESIAN_POINT('Origin',(-14.6542173276259,21.3535257140055,15.));
#27063=CARTESIAN_POINT('',(-18.4844395432208,18.1395876655728,15.));
#27064=CARTESIAN_POINT('',(-14.6542173276259,21.3535257140055,15.));
#27065=CARTESIAN_POINT('Origin',(1.91511110779744,1.60696902421635,0.));
#27066=CARTESIAN_POINT('Origin',(-1.91511110779744,-1.60696902421635,0.));
#27067=CARTESIAN_POINT('Origin',(-23.4120199476077,6.6667373193623,7.5));
#27068=CARTESIAN_POINT('',(-24.2802608359423,1.74269855430126,7.5));
#27069=CARTESIAN_POINT('Origin',(-23.4120199476077,6.6667373193623,7.5));
#27070=CARTESIAN_POINT('',(-23.4120199476077,6.6667373193623,7.5));
#27071=CARTESIAN_POINT('Origin',(-24.9515635041713,6.93820038636033,15.));
#27072=CARTESIAN_POINT('',(-25.8198043925059,2.01416162129929,15.));
#27073=CARTESIAN_POINT('',(-24.9515635041713,6.93820038636033,15.));
#27074=CARTESIAN_POINT('Origin',(0.434120444167318,2.46201938253052,0.));
#27075=CARTESIAN_POINT('Origin',(-0.434120444167318,-2.46201938253052,0.));
#27076=CARTESIAN_POINT('Origin',(-22.2199439289764,-9.94193926282494,7.5));
#27077=CARTESIAN_POINT('',(-22.2199439289764,-9.94193926282494,7.5));
#27078=CARTESIAN_POINT('Origin',(-23.5737958113755,-10.7235860115709,15.));
#27079=CARTESIAN_POINT('',(-21.0737958113755,-15.0537130304931,15.));
#27080=CARTESIAN_POINT('',(-23.5737958113755,-10.7235860115709,15.));
#27081=CARTESIAN_POINT('Origin',(-1.25000000000001,2.16506350946109,0.));
#27082=CARTESIAN_POINT('Origin',(1.25000000000001,-2.16506350946109,0.));
#27083=CARTESIAN_POINT('Origin',(-11.1655870648799,-23.3676873353049,15.));
#27084=CARTESIAN_POINT('',(-6.46712396095037,-25.0777880519332,15.));
#27085=CARTESIAN_POINT('',(-11.1655870648799,-23.3676873353049,15.));
#27086=CARTESIAN_POINT('Origin',(-2.34923155196478,0.855050358314158,0.));
#27087=CARTESIAN_POINT('Origin',(2.34923155196478,-0.855050358314158,0.));
#27088=CARTESIAN_POINT('Origin',(6.4671239609507,-25.0777880519331,15.));
#27089=CARTESIAN_POINT('',(11.1655870648802,-23.3676873353048,15.));
#27090=CARTESIAN_POINT('',(6.4671239609507,-25.0777880519331,15.));
#27091=CARTESIAN_POINT('Origin',(-2.34923155196477,-0.855050358314189,0.));
#27092=CARTESIAN_POINT('Origin',(2.34923155196477,0.855050358314189,0.));
#27093=CARTESIAN_POINT('Origin',(21.0737958113757,-15.0537130304928,15.));
#27094=CARTESIAN_POINT('',(23.5737958113756,-10.7235860115706,15.));
#27095=CARTESIAN_POINT('',(21.0737958113757,-15.0537130304928,15.));
#27096=CARTESIAN_POINT('Origin',(-1.24999999999998,-2.16506350946111,0.));
#27097=CARTESIAN_POINT('Origin',(1.24999999999998,2.16506350946111,0.));
#27098=CARTESIAN_POINT('Origin',(25.8198043925059,2.01416162129963,15.));
#27099=CARTESIAN_POINT('',(24.9515635041712,6.93820038636067,15.));
#27100=CARTESIAN_POINT('',(25.8198043925059,2.01416162129963,15.));
#27101=CARTESIAN_POINT('Origin',(0.434120444167351,-2.46201938253052,0.));
#27102=CARTESIAN_POINT('Origin',(-0.434120444167351,2.46201938253052,0.));
#27103=CARTESIAN_POINT('Origin',(18.4844395432205,18.139587665573,15.));
#27104=CARTESIAN_POINT('',(14.6542173276256,21.3535257140057,15.));
#27105=CARTESIAN_POINT('',(18.4844395432205,18.139587665573,15.));
#27106=CARTESIAN_POINT('Origin',(1.91511110779746,-1.60696902421633,0.));
#27107=CARTESIAN_POINT('Origin',(-1.91511110779746,1.60696902421633,0.));
#27108=CARTESIAN_POINT('Ctrl Pts',(203.999999992307,-0.00177162224216467,
-4.99999968613545));
#27109=CARTESIAN_POINT('Ctrl Pts',(199.974620125013,-0.00177162224216467,
-4.99999968613545));
#27110=CARTESIAN_POINT('Ctrl Pts',(204.000011327375,1.30344668978613,-5.00046215692299));
#27111=CARTESIAN_POINT('Ctrl Pts',(199.974631460081,1.30344668978613,-5.00046215692299));
#27112=CARTESIAN_POINT('Ctrl Pts',(203.985401744253,2.60919356973883,-4.46008193194717));
#27113=CARTESIAN_POINT('Ctrl Pts',(199.960021876959,2.60919356973883,-4.46008193194717));
#27114=CARTESIAN_POINT('Ctrl Pts',(203.953438052627,4.45501092726816,-2.61784253956751));
#27115=CARTESIAN_POINT('Ctrl Pts',(199.928058185333,4.45501092726816,-2.61784253956751));
#27116=CARTESIAN_POINT('Ctrl Pts',(203.938749239315,4.99865586979689,-1.32397596744565));
#27117=CARTESIAN_POINT('Ctrl Pts',(199.913369372021,4.99865586979689,-1.32397596744565));
#27118=CARTESIAN_POINT('Ctrl Pts',(203.938683457647,5.00133895697019,1.31380421087806));
#27119=CARTESIAN_POINT('Ctrl Pts',(199.913303590353,5.00133895697019,1.31380421087806));
#27120=CARTESIAN_POINT('Ctrl Pts',(203.953309177856,4.46081412818035,2.60877766178233));
#27121=CARTESIAN_POINT('Ctrl Pts',(199.927929310562,4.46081412818035,2.60877766178233));
#27122=CARTESIAN_POINT('Ctrl Pts',(203.985313878591,2.61589547515511,4.45664385360227));
#27123=CARTESIAN_POINT('Ctrl Pts',(199.959934011297,2.61589547515511,4.45664385360227));
#27124=CARTESIAN_POINT('Ctrl Pts',(204.,1.32135029102454,5.));
#27125=CARTESIAN_POINT('Ctrl Pts',(199.974620132706,1.32135029102454,5.));
#27126=CARTESIAN_POINT('Ctrl Pts',(204.,2.16840434497101E-16,5.));
#27127=CARTESIAN_POINT('Ctrl Pts',(199.974620132706,2.16840434497101E-16,
5.));
#27128=CARTESIAN_POINT('Origin',(-175.75628980623,-72.1784357931688,12.5));
#27129=CARTESIAN_POINT('Origin',(-175.75628980623,72.1784357931688,7.5));
#27130=CARTESIAN_POINT('Ctrl Pts',(-204.,1.12757025938492E-14,5.));
#27131=CARTESIAN_POINT('Ctrl Pts',(-199.97462301248,1.12757025938492E-14,
5.));
#27132=CARTESIAN_POINT('Ctrl Pts',(-204.,-1.32135029102452,5.));
#27133=CARTESIAN_POINT('Ctrl Pts',(-199.97462301248,-1.32135029102452,5.));
#27134=CARTESIAN_POINT('Ctrl Pts',(-203.985345962115,-2.61339289425714,
4.45784180166548));
#27135=CARTESIAN_POINT('Ctrl Pts',(-199.959968974596,-2.61339289425714,
4.45784180166548));
#27136=CARTESIAN_POINT('Ctrl Pts',(-203.95336383834,-4.45831456152484,2.61258630841651));
#27137=CARTESIAN_POINT('Ctrl Pts',(-199.92798685082,-4.45831456152484,2.61258630841651));
#27138=CARTESIAN_POINT('Ctrl Pts',(-203.938733312599,-4.99930548519225,
1.30702665821118));
#27139=CARTESIAN_POINT('Ctrl Pts',(-199.913356325079,-4.99930548519225,
1.30702665821118));
#27140=CARTESIAN_POINT('Ctrl Pts',(-203.938699292213,-5.00069310016037,
-1.30170754686162));
#27141=CARTESIAN_POINT('Ctrl Pts',(-199.913322304693,-5.00069310016037,
-1.30170754686162));
#27142=CARTESIAN_POINT('Ctrl Pts',(-203.953150206633,-4.47024776275285,
-2.59986968375127));
#27143=CARTESIAN_POINT('Ctrl Pts',(-199.927773219114,-4.47024776275285,
-2.59986968375127));
#27144=CARTESIAN_POINT('Ctrl Pts',(-203.985508343536,-2.60441550046637,
-4.46760084763805));
#27145=CARTESIAN_POINT('Ctrl Pts',(-199.960131356017,-2.60441550046637,
-4.46760084763805));
#27146=CARTESIAN_POINT('Ctrl Pts',(-203.99998865724,-1.30698993427041,-4.99953721534794));
#27147=CARTESIAN_POINT('Ctrl Pts',(-199.97461166972,-1.30698993427041,-4.99953721534794));
#27148=CARTESIAN_POINT('Ctrl Pts',(-204.000000269508,0.0301477011414563,
-5.00001099593282));
#27149=CARTESIAN_POINT('Ctrl Pts',(-199.974623281988,0.0301477011414563,
-5.00001099593282));
#27150=CARTESIAN_POINT('Ctrl Pts',(-203.999991802598,0.0620673406376593,
-4.9996988521178));
#27151=CARTESIAN_POINT('Ctrl Pts',(-199.974614815078,0.0620673406376593,
-4.9996988521178));
#27152=CARTESIAN_POINT('Ctrl Pts',(-203.999974785344,0.0939816893050483,
-4.9990655962846));
#27153=CARTESIAN_POINT('Ctrl Pts',(-199.974597797824,0.0939816893050483,
-4.9990655962846));
#27154=CARTESIAN_POINT('Origin',(2.47860448411075,13.6831560121067,-15.));
#27155=CARTESIAN_POINT('',(2.47860448411075,21.6999127067652,-15.));
#27156=CARTESIAN_POINT('Origin',(-2.0402937480676,13.6831560121067,-15.));
#27157=CARTESIAN_POINT('',(-2.0402937480676,21.6999127067652,-15.));
#27158=CARTESIAN_POINT('Origin',(-2.0402937480676,21.6999127067652,-15.));
#27159=CARTESIAN_POINT('',(0.,0.,0.));
#27160=CARTESIAN_POINT('Origin',(0.,0.,0.));
#27161=CARTESIAN_POINT('',(1.27363267111325E-14,208.,-1.71450551880629E-15));
#27162=CARTESIAN_POINT('',(0.,222.,-14.));
#27163=CARTESIAN_POINT('Origin',(1.35935794705356E-14,222.,0.));
#27164=CARTESIAN_POINT('',(-183.924299418847,97.1383141879995,-2.45234074816238E-11));
#27165=CARTESIAN_POINT('Origin',(0.,0.,-1.71450551880629E-15));
#27166=CARTESIAN_POINT('',(-188.965207680627,91.9372213898726,7.4447346109596));
#27167=CARTESIAN_POINT('Ctrl Pts',(-188.965207680626,91.9372213898729,7.44473461095943));
#27168=CARTESIAN_POINT('Ctrl Pts',(-188.777281065684,92.1417492337039,7.31811198115176));
#27169=CARTESIAN_POINT('Ctrl Pts',(-188.589786144602,92.3445422191641,7.18727696952707));
#27170=CARTESIAN_POINT('Ctrl Pts',(-188.402949359252,92.5454067376809,7.05154332610887));
#27171=CARTESIAN_POINT('Ctrl Pts',(-188.216112573901,92.7462712561977,6.91580968269067));
#27172=CARTESIAN_POINT('Ctrl Pts',(-188.029934009438,92.9452072423305,6.77517683974821));
#27173=CARTESIAN_POINT('Ctrl Pts',(-187.84463499754,93.142030410138,6.62901215662966));
#27174=CARTESIAN_POINT('Ctrl Pts',(-187.685431029225,93.3111356258137,6.50343135972319));
#27175=CARTESIAN_POINT('Ctrl Pts',(-187.526731368968,93.478830345021,6.37369884055212));
#27176=CARTESIAN_POINT('Ctrl Pts',(-187.368931721517,93.644742838303,6.23917845532948));
#27177=CARTESIAN_POINT('Ctrl Pts',(-187.358712366937,93.6554875936023,6.23046670256522));
#27178=CARTESIAN_POINT('Ctrl Pts',(-187.348496782088,93.6662248798462,6.22173488584732));
#27179=CARTESIAN_POINT('Ctrl Pts',(-187.338285072337,93.6769545984829,6.21298283941028));
#27180=CARTESIAN_POINT('Ctrl Pts',(-187.204548187013,93.8174755480478,6.09836232440827));
#27181=CARTESIAN_POINT('Ctrl Pts',(-187.071431813471,93.9567739444096,5.98026061216412));
#27182=CARTESIAN_POINT('Ctrl Pts',(-186.939063717966,94.0947139001685,5.85818571601648));
#27183=CARTESIAN_POINT('Ctrl Pts',(-186.869499901573,94.167205913588,5.79403131665466));
#27184=CARTESIAN_POINT('Ctrl Pts',(-186.79969674014,94.2397787170827,5.72835556874943));
#27185=CARTESIAN_POINT('Ctrl Pts',(-186.730077654463,94.311986609344,5.66143525552039));
#27186=CARTESIAN_POINT('Ctrl Pts',(-186.667223476599,94.3771780386651,5.60101760956244));
#27187=CARTESIAN_POINT('Ctrl Pts',(-186.604587356584,94.4420013140829,5.53968086297713));
#27188=CARTESIAN_POINT('Ctrl Pts',(-186.542485785002,94.50613245851,5.47761211877966));
#27189=CARTESIAN_POINT('Ctrl Pts',(-186.436000166469,94.6160981873572,5.37118278939107));
#27190=CARTESIAN_POINT('Ctrl Pts',(-186.330692100467,94.7244995729387,5.26228082287464));
#27191=CARTESIAN_POINT('Ctrl Pts',(-186.226759940933,94.831157452253,5.15054882323236));
#27192=CARTESIAN_POINT('Ctrl Pts',(-186.125678797888,94.9348895444588,5.04188180150126));
#27193=CARTESIAN_POINT('Ctrl Pts',(-186.02589914915,95.0369724528684,4.93053778166716));
#27194=CARTESIAN_POINT('Ctrl Pts',(-185.927591324053,95.1372549667413,4.81623371046665));
#27195=CARTESIAN_POINT('Ctrl Pts',(-185.878492805196,95.1873397173047,4.75914608199233));
#27196=CARTESIAN_POINT('Ctrl Pts',(-185.829761217654,95.2369756002562,4.70132084032866));
#27197=CARTESIAN_POINT('Ctrl Pts',(-185.781416555225,95.2861451237541,4.64272728542119));
#27198=CARTESIAN_POINT('Ctrl Pts',(-185.737559874666,95.3307500910229,4.58957314820614));
#27199=CARTESIAN_POINT('Ctrl Pts',(-185.694016468188,95.3749718553161,4.53577438997125));
#27200=CARTESIAN_POINT('Ctrl Pts',(-185.650807802727,95.41879168514,4.4813195101232));
#27201=CARTESIAN_POINT('Ctrl Pts',(-185.574087130878,95.4965975314552,4.38463022516696));
#27202=CARTESIAN_POINT('Ctrl Pts',(-185.498348272351,95.5732099457179,4.28567472753969));
#27203=CARTESIAN_POINT('Ctrl Pts',(-185.424001069689,95.6482394066019,4.18453965879523));
#27204=CARTESIAN_POINT('Ctrl Pts',(-185.352087703078,95.7208126969739,4.08671535585732));
#27205=CARTESIAN_POINT('Ctrl Pts',(-185.281476519291,95.7919048404079,3.98685192836821));
#27206=CARTESIAN_POINT('Ctrl Pts',(-185.212508038807,95.8611936177919,3.88505147091736));
#27207=CARTESIAN_POINT('Ctrl Pts',(-185.188395255985,95.8854183829225,3.84945996151216));
#27208=CARTESIAN_POINT('Ctrl Pts',(-185.164482979243,95.9094230017288,3.81363189217638));
#27209=CARTESIAN_POINT('Ctrl Pts',(-185.140784795543,95.9331946623266,3.77757231362429));
#27210=CARTESIAN_POINT('Ctrl Pts',(-185.121628056577,95.9524107973109,3.74842307829493));
#27211=CARTESIAN_POINT('Ctrl Pts',(-185.102604574441,95.9714814439119,3.71911920337178));
#27212=CARTESIAN_POINT('Ctrl Pts',(-185.083719917007,95.9904016355523,3.68965406509349));
#27213=CARTESIAN_POINT('Ctrl Pts',(-185.024451423954,96.0497816508219,3.59717929559146));
#27214=CARTESIAN_POINT('Ctrl Pts',(-184.966549837208,96.1076881079189,3.50312319977729));
#27215=CARTESIAN_POINT('Ctrl Pts',(-184.91017752504,96.1639721188239,3.40730682859391));
#27216=CARTESIAN_POINT('Ctrl Pts',(-184.854918825039,96.219144261918,3.31338327096742));
#27217=CARTESIAN_POINT('Ctrl Pts',(-184.801129614601,96.2727574049647,3.21776823030466));
#27218=CARTESIAN_POINT('Ctrl Pts',(-184.748944154795,96.3246902126642,3.12033555929367));
#27219=CARTESIAN_POINT('Ctrl Pts',(-184.722937793693,96.3505706658611,3.07178047834085));
#27220=CARTESIAN_POINT('Ctrl Pts',(-184.697329423299,96.3760341107952,3.02277466583946));
#27221=CARTESIAN_POINT('Ctrl Pts',(-184.672133835317,96.4010673582064,2.97330663101595));
#27222=CARTESIAN_POINT('Ctrl Pts',(-184.627607521379,96.4453067795653,2.88588540274296));
#27223=CARTESIAN_POINT('Ctrl Pts',(-184.58424172121,96.4883286304064,2.79669596755631));
#27224=CARTESIAN_POINT('Ctrl Pts',(-184.54235398425,96.5298308010085,2.70593977270456));
#27225=CARTESIAN_POINT('Ctrl Pts',(-184.526333540261,96.5457037807351,2.67122902818081));
#27226=CARTESIAN_POINT('Ctrl Pts',(-184.510528921791,96.561354839112,2.63628916907188));
#27227=CARTESIAN_POINT('Ctrl Pts',(-184.49495645186,96.5767684840588,2.60113170275939));
#27228=CARTESIAN_POINT('Ctrl Pts',(-184.457448604398,96.6138937856985,2.51645143756278));
#27229=CARTESIAN_POINT('Ctrl Pts',(-184.42119837209,96.6497332749268,2.43030849578046));
#27230=CARTESIAN_POINT('Ctrl Pts',(-184.386467350968,96.6840359323964,2.34293783062457));
#27231=CARTESIAN_POINT('Ctrl Pts',(-184.352937166828,96.7171525637043,2.25858803621967));
#27232=CARTESIAN_POINT('Ctrl Pts',(-184.32082314254,96.7488366313688,2.17309415060979));
#27233=CARTESIAN_POINT('Ctrl Pts',(-184.290328389036,96.7788942509748,2.08668618679845));
#27234=CARTESIAN_POINT('Ctrl Pts',(-184.283436100126,96.7856877408207,2.06715664212894));
#27235=CARTESIAN_POINT('Ctrl Pts',(-184.27662638795,96.7923982854362,2.04758047426811));
#27236=CARTESIAN_POINT('Ctrl Pts',(-184.269901344592,96.7990238955975,2.02796046082246));
#27237=CARTESIAN_POINT('Ctrl Pts',(-184.26623686533,96.8026341936638,2.01726950634743));
#27238=CARTESIAN_POINT('Ctrl Pts',(-184.262597332157,96.8062194864247,2.00656547941313));
#27239=CARTESIAN_POINT('Ctrl Pts',(-184.258983022864,96.8097795163212,1.99584840652776));
#27240=CARTESIAN_POINT('Ctrl Pts',(-184.223537518536,96.8446927030049,1.89074615255131));
#27241=CARTESIAN_POINT('Ctrl Pts',(-184.190473176187,96.8772201529816,1.78424485552327));
#27242=CARTESIAN_POINT('Ctrl Pts',(-184.159960059398,96.9072126758638,1.67612419944574));
#27243=CARTESIAN_POINT('Ctrl Pts',(-184.143137275991,96.9237484404584,1.61651408516027));
#27244=CARTESIAN_POINT('Ctrl Pts',(-184.127089415644,96.9395141816105,1.55641233920697));
#27245=CARTESIAN_POINT('Ctrl Pts',(-184.111841067988,96.9544884398172,1.49578619414718));
#27246=CARTESIAN_POINT('Ctrl Pts',(-184.10013259563,96.9659864520781,1.44923429490751));
#27247=CARTESIAN_POINT('Ctrl Pts',(-184.088901899494,96.97701152717,1.40233382499999));
#27248=CARTESIAN_POINT('Ctrl Pts',(-184.078180757733,96.9875336813599,1.35519738700399));
#27249=CARTESIAN_POINT('Ctrl Pts',(-184.058107442441,97.0072344299651,1.26694329964282));
#27250=CARTESIAN_POINT('Ctrl Pts',(-184.039793616161,97.0251959100348,1.17773537467592));
#27251=CARTESIAN_POINT('Ctrl Pts',(-184.023436891388,97.0412305639008,1.08817980520529));
#27252=CARTESIAN_POINT('Ctrl Pts',(-184.013337630761,97.0511309657662,1.03288480885195));
#27253=CARTESIAN_POINT('Ctrl Pts',(-184.003984328087,97.060296937738,0.977456098654038));
#27254=CARTESIAN_POINT('Ctrl Pts',(-183.995422776363,97.06868494987,0.922026700139618));
#27255=CARTESIAN_POINT('Ctrl Pts',(-183.976848898345,97.0868823420241,0.801775264428186));
#27256=CARTESIAN_POINT('Ctrl Pts',(-183.961821282879,97.1015955688319,0.68091917253188));
#27257=CARTESIAN_POINT('Ctrl Pts',(-183.950437303463,97.1127380434133,0.559199366684126));
#27258=CARTESIAN_POINT('Ctrl Pts',(-183.943134370342,97.1198860488431,0.481114931601442));
#27259=CARTESIAN_POINT('Ctrl Pts',(-183.93733152959,97.1255639515528,0.402674791403003));
#27260=CARTESIAN_POINT('Ctrl Pts',(-183.9330622763,97.1297411343775,0.32380729739441));
#27261=CARTESIAN_POINT('Ctrl Pts',(-183.927831946245,97.1348586674432,0.227185477057826));
#27262=CARTESIAN_POINT('Ctrl Pts',(-183.924970282477,97.1376584995943,0.129411875784403));
#27263=CARTESIAN_POINT('Ctrl Pts',(-183.924458161665,97.1381595218518,0.0316528433418993));
#27264=CARTESIAN_POINT('Ctrl Pts',(-183.924402886243,97.138213599358,0.0211012867892161));
#27265=CARTESIAN_POINT('Ctrl Pts',(-183.924375001864,97.138240877262,0.0105498589472018));
#27266=CARTESIAN_POINT('Ctrl Pts',(-183.924374498502,97.1382413655954,-7.00888014293355E-10));
#27267=CARTESIAN_POINT('',(-183.924299418846,-97.1383141879995,1.6286382377323E-15));
#27268=CARTESIAN_POINT('Ctrl Pts',(-183.924299418846,-97.1383141879995,
1.6286382377323E-15));
#27269=CARTESIAN_POINT('Ctrl Pts',(-183.924299418847,-97.1383141879996,
0.289606573667191));
#27270=CARTESIAN_POINT('Ctrl Pts',(-183.945294598411,-97.1177882275971,
0.576128192439725));
#27271=CARTESIAN_POINT('Ctrl Pts',(-184.026954906122,-97.0378030821182,
1.14333145788899));
#27272=CARTESIAN_POINT('Ctrl Pts',(-184.087299204572,-96.9786517847449,
1.42056425530318));
#27273=CARTESIAN_POINT('Ctrl Pts',(-184.239213583142,-96.8293094810531,
1.95495869016732));
#27274=CARTESIAN_POINT('Ctrl Pts',(-184.331762894336,-96.7381490066639,
2.21530983652599));
#27275=CARTESIAN_POINT('Ctrl Pts',(-184.539595228575,-96.5326824648098,
2.71171918629039));
#27276=CARTESIAN_POINT('Ctrl Pts',(-184.654706063204,-96.4185488213364,
2.94816573920908));
#27277=CARTESIAN_POINT('Ctrl Pts',(-185.02647179182,-96.0483938637497,3.62930814728168));
#27278=CARTESIAN_POINT('Ctrl Pts',(-185.311549180074,-95.7625411976457,
4.04843931623329));
#27279=CARTESIAN_POINT('Ctrl Pts',(-185.908081548002,-95.1582117642484,
4.81028372456617));
#27280=CARTESIAN_POINT('Ctrl Pts',(-186.221658835681,-94.8376773560741,
5.15691217997208));
#27281=CARTESIAN_POINT('Ctrl Pts',(-186.868145715832,-94.1697219232036,
5.80304524490739));
#27282=CARTESIAN_POINT('Ctrl Pts',(-187.201193142186,-93.8221709116559,
6.10227777090564));
#27283=CARTESIAN_POINT('Ctrl Pts',(-187.880549907623,-93.1052140686194,
6.66488432085835));
#27284=CARTESIAN_POINT('Ctrl Pts',(-188.22814505543,-92.7344219550961,6.92900726524237));
#27285=CARTESIAN_POINT('Ctrl Pts',(-189.275208253741,-91.6044438981369,
7.67158459471431));
#27286=CARTESIAN_POINT('Ctrl Pts',(-189.976354544114,-90.8305882749372,
8.10040126241789));
#27287=CARTESIAN_POINT('Ctrl Pts',(-191.374588317242,-89.250261707686,8.87382214052879));
#27288=CARTESIAN_POINT('Ctrl Pts',(-192.071836977406,-88.4436449005057,
9.21763122303672));
#27289=CARTESIAN_POINT('Ctrl Pts',(-193.457278361193,-86.8015935109936,
9.84360712907318));
#27290=CARTESIAN_POINT('Ctrl Pts',(-194.145522657778,-85.9661135276441,
10.1255231834183));
#27291=CARTESIAN_POINT('Ctrl Pts',(-196.19191597214,-83.4197910447744,10.8995122536796));
#27292=CARTESIAN_POINT('Ctrl Pts',(-197.531515647658,-81.6692498423691,
11.3208437569989));
#27293=CARTESIAN_POINT('Ctrl Pts',(-199.492190335423,-78.9710560946796,
11.8586418616589));
#27294=CARTESIAN_POINT('Ctrl Pts',(-200.138798925329,-78.0578863331849,
12.0220836807334));
#27295=CARTESIAN_POINT('Ctrl Pts',(-201.40602210199,-76.2205466037287,12.3199232325791));
#27296=CARTESIAN_POINT('Ctrl Pts',(-202.027379911037,-75.2954459129312,
12.4545571141892));
#27297=CARTESIAN_POINT('Ctrl Pts',(-203.854832722202,-72.5012481746631,
12.8226747946999));
#27298=CARTESIAN_POINT('Ctrl Pts',(-205.024317580872,-70.6132750985836,
13.0206893865685));
#27299=CARTESIAN_POINT('Ctrl Pts',(-208.387244631561,-64.8761223846278,
13.5122485336218));
#27300=CARTESIAN_POINT('Ctrl Pts',(-210.435425840902,-60.9539161091157,
13.7050519148717));
#27301=CARTESIAN_POINT('Ctrl Pts',(-214.144176955874,-52.9203842766436,
13.9447223410129));
#27302=CARTESIAN_POINT('Ctrl Pts',(-215.804813106923,-48.8090196665873,
13.9900872820394));
#27303=CARTESIAN_POINT('Ctrl Pts',(-217.998369105242,-42.4995152895031,
14.0027740092237));
#27304=CARTESIAN_POINT('Ctrl Pts',(-218.679912382467,-40.3725573743037,
13.9975347191773));
#27305=CARTESIAN_POINT('Ctrl Pts',(-219.62616267774,-37.1459345955272,13.980864955456));
#27306=CARTESIAN_POINT('Ctrl Pts',(-219.929225739207,-36.0631092234961,
13.9738214451819));
#27307=CARTESIAN_POINT('Ctrl Pts',(-220.508095214681,-33.8911509216661,
13.9576271630892));
#27308=CARTESIAN_POINT('Ctrl Pts',(-220.783424005549,-32.8039498686341,
13.9484949198543));
#27309=CARTESIAN_POINT('Ctrl Pts',(-222.090385807589,-27.3619003043185,
13.8996044768986));
#27310=CARTESIAN_POINT('Ctrl Pts',(-222.913500587235,-22.9889613912764,
13.8509457895095));
#27311=CARTESIAN_POINT('Ctrl Pts',(-224.127738137291,-14.2054494124102,
13.7709601634318));
#27312=CARTESIAN_POINT('Ctrl Pts',(-224.518828150004,-9.79487372996352,
13.7395801077819));
#27313=CARTESIAN_POINT('Ctrl Pts',(-224.869105640044,-0.936019490422407,
13.7117102244513));
#27314=CARTESIAN_POINT('Ctrl Pts',(-224.828321321409,3.51225676594121,13.7152551483673));
#27315=CARTESIAN_POINT('Ctrl Pts',(-224.499599127585,9.09684225070298,13.7409136885715));
#27316=CARTESIAN_POINT('Ctrl Pts',(-224.4199349447,10.2149739885714,13.7470594015732));
#27317=CARTESIAN_POINT('Ctrl Pts',(-224.23243573416,12.4536946433225,13.7611695346538));
#27318=CARTESIAN_POINT('Ctrl Pts',(-224.124563005179,13.5740681295282,13.7691356336449));
#27319=CARTESIAN_POINT('Ctrl Pts',(-223.76071604259,16.9182868017048,13.7951450599868));
#27320=CARTESIAN_POINT('Ctrl Pts',(-223.464013321503,19.1321332304902,13.8153704223117));
#27321=CARTESIAN_POINT('Ctrl Pts',(-222.415051088304,25.7277907019174,13.8795349289317));
#27322=CARTESIAN_POINT('Ctrl Pts',(-221.504313463055,30.0638296946454,13.9274520583673));
#27323=CARTESIAN_POINT('Ctrl Pts',(-219.269264018172,38.6163649455757,13.9942669977442));
#27324=CARTESIAN_POINT('Ctrl Pts',(-217.944936174541,42.8328570669653,14.0133729245824));
#27325=CARTESIAN_POINT('Ctrl Pts',(-214.88002904003,51.1453899765955,13.9654070644487));
#27326=CARTESIAN_POINT('Ctrl Pts',(-213.13949100334,55.2414444523707,13.8990836182993));
#27327=CARTESIAN_POINT('Ctrl Pts',(-210.694370828089,60.283416978766,13.7075079551512));
#27328=CARTESIAN_POINT('Ctrl Pts',(-210.191194888016,61.2891398827893,13.663578611472));
#27329=CARTESIAN_POINT('Ctrl Pts',(-209.16065556682,63.2865110306788,13.5629787339324));
#27330=CARTESIAN_POINT('Ctrl Pts',(-208.633964828839,64.2769408168412,13.5063869810004));
#27331=CARTESIAN_POINT('Ctrl Pts',(-207.020159630544,67.2234096152245,13.3148819803906));
#27332=CARTESIAN_POINT('Ctrl Pts',(-205.899309096341,69.1546564288455,13.1584578298572));
#27333=CARTESIAN_POINT('Ctrl Pts',(-203.570426573057,72.9501257617516,12.7687139843163));
#27334=CARTESIAN_POINT('Ctrl Pts',(-202.362373093814,74.8143635854865,12.5356047498722));
#27335=CARTESIAN_POINT('Ctrl Pts',(-199.862178770943,78.4738596816999,11.9639786153397));
#27336=CARTESIAN_POINT('Ctrl Pts',(-198.569984776825,80.2691602211054,11.6260140633101));
#27337=CARTESIAN_POINT('Ctrl Pts',(-196.57195550953,82.9075286142192,11.0039793996147));
#27338=CARTESIAN_POINT('Ctrl Pts',(-195.89600311974,83.7778708332067,10.7772677458374));
#27339=CARTESIAN_POINT('Ctrl Pts',(-194.525119525015,85.4994949310966,10.2748858952649));
#27340=CARTESIAN_POINT('Ctrl Pts',(-193.83201420713,86.3483748013007,9.99984001499434));
#27341=CARTESIAN_POINT('Ctrl Pts',(-192.443022672674,88.0089491897228,9.39284720135033));
#27342=CARTESIAN_POINT('Ctrl Pts',(-191.745822424016,88.8222836276672,9.06062243030275));
#27343=CARTESIAN_POINT('Ctrl Pts',(-190.352288451153,90.4105500302893,8.31897581534296));
#27344=CARTESIAN_POINT('Ctrl Pts',(-189.655811580761,91.1856103065845,7.91005498091941));
#27345=CARTESIAN_POINT('Ctrl Pts',(-188.965207680627,91.9372213898726,7.4447346109596));
#27346=CARTESIAN_POINT('',(-3.15824218834415E-14,-208.,-1.71450551880629E-15));
#27347=CARTESIAN_POINT('Origin',(0.,0.,-1.71450551880629E-15));
#27348=CARTESIAN_POINT('',(-3.15824218834415E-14,-222.,14.));
#27349=CARTESIAN_POINT('Origin',(-3.15824218834415E-14,-222.,0.));
#27350=CARTESIAN_POINT('Origin',(-3.15824218834415E-14,-222.,0.));
#27351=CARTESIAN_POINT('',(-189.252344883447,-91.6237366354615,-7.63473361656836));
#27352=CARTESIAN_POINT('Ctrl Pts',(-189.252344883447,-91.6237366354615,
-7.63473361656836));
#27353=CARTESIAN_POINT('Ctrl Pts',(-188.666509085829,-92.2653391382624,
-7.2539887318565));
#27354=CARTESIAN_POINT('Ctrl Pts',(-188.089380051022,-92.8849778109279,
-6.83875146569526));
#27355=CARTESIAN_POINT('Ctrl Pts',(-186.968116025761,-94.0679928081637,
-5.90831038164945));
#27356=CARTESIAN_POINT('Ctrl Pts',(-186.423262692469,-94.6320391895917,
-5.39465052751624));
#27357=CARTESIAN_POINT('Ctrl Pts',(-185.655376248049,-95.4148977911641,
-4.49846237685947));
#27358=CARTESIAN_POINT('Ctrl Pts',(-185.406583998279,-95.6663955704661,
-4.17665287330735));
#27359=CARTESIAN_POINT('Ctrl Pts',(-184.940925516141,-96.1338625850361,
-3.47817276299474));
#27360=CARTESIAN_POINT('Ctrl Pts',(-184.726546490054,-96.3473475582936,
-3.10569066952788));
#27361=CARTESIAN_POINT('Ctrl Pts',(-184.354363966567,-96.7160922094891,
-2.29793911795022));
#27362=CARTESIAN_POINT('Ctrl Pts',(-184.201053959324,-96.8669273884385,
-1.87245077917943));
#27363=CARTESIAN_POINT('Ctrl Pts',(-184.038570146028,-97.0264280245017,
-1.19046756850576));
#27364=CARTESIAN_POINT('Ctrl Pts',(-183.995900054248,-97.0682280802022,
-0.955005769387058));
#27365=CARTESIAN_POINT('Ctrl Pts',(-183.9389953264,-97.1239440434863,-0.481662656210902));
#27366=CARTESIAN_POINT('Ctrl Pts',(-183.924299418846,-97.1383141879995,
-0.241197781359841));
#27367=CARTESIAN_POINT('Ctrl Pts',(-183.924299418846,-97.1383141879995,
1.6286382377323E-15));
#27368=CARTESIAN_POINT('Ctrl Pts',(-183.924299418847,97.1383141879995,-2.45234074816238E-11));
#27369=CARTESIAN_POINT('Ctrl Pts',(-183.924299418848,97.1383141879982,-0.289293301043451));
#27370=CARTESIAN_POINT('Ctrl Pts',(-183.945246216988,97.1178352743025,-0.574831380827163));
#27371=CARTESIAN_POINT('Ctrl Pts',(-184.026168974811,97.0385732297218,-1.13882338953088));
#27372=CARTESIAN_POINT('Ctrl Pts',(-184.086353500478,96.9795792606563,-1.41641997278048));
#27373=CARTESIAN_POINT('Ctrl Pts',(-184.237290286536,96.8312023888215,-1.94899521951201));
#27374=CARTESIAN_POINT('Ctrl Pts',(-184.328773586646,96.7410972488276,-2.20734178770506));
#27375=CARTESIAN_POINT('Ctrl Pts',(-184.536045978299,96.5361981324799,-2.70404415625005));
#27376=CARTESIAN_POINT('Ctrl Pts',(-184.650675626616,96.4225494185532,-2.94010876392827));
#27377=CARTESIAN_POINT('Ctrl Pts',(-184.897041418233,96.1772753531742,-3.3928151445005));
#27378=CARTESIAN_POINT('Ctrl Pts',(-185.028806857472,96.0456213657732,-3.60942484353172));
#27379=CARTESIAN_POINT('Ctrl Pts',(-185.306190021303,95.7671972032446,-4.02660699512156));
#27380=CARTESIAN_POINT('Ctrl Pts',(-185.452123042776,95.620101727754,-4.22741942202966));
#27381=CARTESIAN_POINT('Ctrl Pts',(-185.899177016858,95.1672867203483,-4.79996460051786));
#27382=CARTESIAN_POINT('Ctrl Pts',(-186.211874696161,94.8477060015223,-5.14633171366901));
#27383=CARTESIAN_POINT('Ctrl Pts',(-187.177253870719,93.8505055701753,-6.11354637057988));
#27384=CARTESIAN_POINT('Ctrl Pts',(-187.856598791335,93.134972043538,-6.66377670847504));
#27385=CARTESIAN_POINT('Ctrl Pts',(-188.899602703674,92.0099908210452,-7.40602386987046));
#27386=CARTESIAN_POINT('Ctrl Pts',(-189.251093155014,91.6265899532315,-7.63854891641251));
#27387=CARTESIAN_POINT('Ctrl Pts',(-189.951287505344,90.8538465649765,-8.07489972933164));
#27388=CARTESIAN_POINT('Ctrl Pts',(-190.301206659029,90.4632019265966,-8.27956354245871));
#27389=CARTESIAN_POINT('Ctrl Pts',(-191.348977896207,89.2796407946467,-8.86065506893184));
#27390=CARTESIAN_POINT('Ctrl Pts',(-192.044773452492,88.4751580400445,-9.20456317412189));
#27391=CARTESIAN_POINT('Ctrl Pts',(-193.426080088475,86.8391100951027,-9.83031641121458));
#27392=CARTESIAN_POINT('Ctrl Pts',(-194.111639716675,86.0075020766135,-10.1118965188247));
#27393=CARTESIAN_POINT('Ctrl Pts',(-196.148613709987,83.4751543078266,-10.8846927099913));
#27394=CARTESIAN_POINT('Ctrl Pts',(-197.480133504116,81.7370594032411,-11.305004133147));
#27395=CARTESIAN_POINT('Ctrl Pts',(-199.427277956411,79.061736809832,-11.8416503383128));
#27396=CARTESIAN_POINT('Ctrl Pts',(-200.068037672566,78.1585401083653,-12.0045286228002));
#27397=CARTESIAN_POINT('Ctrl Pts',(-201.331792808165,76.3299028888316,-12.3033005273701));
#27398=CARTESIAN_POINT('Ctrl Pts',(-201.955766490901,75.4029324575626,-12.4393616147252));
#27399=CARTESIAN_POINT('Ctrl Pts',(-203.789380826525,72.6050223527821,-12.8109057765609));
#27400=CARTESIAN_POINT('Ctrl Pts',(-204.962444257487,70.7149876206329,-13.0106557132063));
#27401=CARTESIAN_POINT('Ctrl Pts',(-208.334885204917,64.97284066522,-13.5064989325318));
#27402=CARTESIAN_POINT('Ctrl Pts',(-210.387791961828,61.0488867819828,-13.7009628268141));
#27403=CARTESIAN_POINT('Ctrl Pts',(-214.104196849767,53.0150029671012,-13.9431260054544));
#27404=CARTESIAN_POINT('Ctrl Pts',(-215.767750838602,48.9050361592617,-13.989284646881));
#27405=CARTESIAN_POINT('Ctrl Pts',(-217.965171860694,42.6001126302614,-14.002865883644));
#27406=CARTESIAN_POINT('Ctrl Pts',(-218.647916793637,40.4750969194813,-13.9978706752266));
#27407=CARTESIAN_POINT('Ctrl Pts',(-219.595939962548,37.2520377674546,-13.9815031003));
#27408=CARTESIAN_POINT('Ctrl Pts',(-219.899368743631,36.171187315868,-13.9745517151795));
#27409=CARTESIAN_POINT('Ctrl Pts',(-220.477440402961,34.0097240519904,-13.9585793089129));
#27410=CARTESIAN_POINT('Ctrl Pts',(-220.752532941888,32.9276497263176,-13.9495525121151));
#27411=CARTESIAN_POINT('Ctrl Pts',(-222.059068051356,27.510631885896,-13.9011404780045));
#27412=CARTESIAN_POINT('Ctrl Pts',(-222.884242784183,23.1557959145204,-13.8526891852329));
#27413=CARTESIAN_POINT('Ctrl Pts',(-224.106142919279,14.404638181653,-13.772559117181));
#27414=CARTESIAN_POINT('Ctrl Pts',(-224.502841203057,10.0083140242484,-13.7408321408321));
#27415=CARTESIAN_POINT('Ctrl Pts',(-224.866867117856,1.17400800753462,-13.711907328236));
#27416=CARTESIAN_POINT('Ctrl Pts',(-224.83422743905,-3.26397087488992,-13.7147485874252));
#27417=CARTESIAN_POINT('Ctrl Pts',(-224.453183725159,-9.95315272494675,
-13.7445574981991));
#27418=CARTESIAN_POINT('Ctrl Pts',(-224.269875506322,-12.1940962642215,
-13.7586615908191));
#27419=CARTESIAN_POINT('Ctrl Pts',(-223.795577148681,-16.6370922798083,
-13.7927293726463));
#27420=CARTESIAN_POINT('Ctrl Pts',(-223.504633439409,-18.8435115295463,
-13.8126877638542));
#27421=CARTESIAN_POINT('Ctrl Pts',(-222.473806565301,-25.4184761287494,
-13.8762990186828));
#27422=CARTESIAN_POINT('Ctrl Pts',(-221.576298994197,-29.7428330952291,
-13.9241751615609));
#27423=CARTESIAN_POINT('Ctrl Pts',(-219.369230163102,-38.2759802604658,
-13.992319185983));
#27424=CARTESIAN_POINT('Ctrl Pts',(-218.059656539427,-42.4847672627358,
-14.0127887068107));
#27425=CARTESIAN_POINT('Ctrl Pts',(-215.025133999908,-50.7857678762348,
-13.9698621357405));
#27426=CARTESIAN_POINT('Ctrl Pts',(-213.300229963115,-54.8779950418535,
-13.907191527293));
#27427=CARTESIAN_POINT('Ctrl Pts',(-210.874797903038,-59.9176309101772,
-13.7225218764077));
#27428=CARTESIAN_POINT('Ctrl Pts',(-210.375538180112,-60.9230450669806,
-13.6800873300562));
#27429=CARTESIAN_POINT('Ctrl Pts',(-209.354416026681,-62.9170286488566,
-13.5829151958296));
#27430=CARTESIAN_POINT('Ctrl Pts',(-208.832334628704,-63.9061429936345,
-13.5281755289986));
#27431=CARTESIAN_POINT('Ctrl Pts',(-207.231970951578,-66.8497997256187,
-13.3426795325515));
#27432=CARTESIAN_POINT('Ctrl Pts',(-206.119569880797,-68.7806813058041,
-13.1908611905979));
#27433=CARTESIAN_POINT('Ctrl Pts',(-203.806019801973,-72.5784926687438,
-12.8117980747563));
#27434=CARTESIAN_POINT('Ctrl Pts',(-202.604853069669,-74.4454352778335,
-12.5847577915574));
#27435=CARTESIAN_POINT('Ctrl Pts',(-200.116163488173,-78.1135836520715,
-12.0271908520484));
#27436=CARTESIAN_POINT('Ctrl Pts',(-198.82859706036,-79.9148244022689,-11.6971965579858));
#27437=CARTESIAN_POINT('Ctrl Pts',(-196.835024756913,-82.5648480465928,
-11.0892859689757));
#27438=CARTESIAN_POINT('Ctrl Pts',(-196.161413841412,-83.4377758103841,
-10.8679626155705));
#27439=CARTESIAN_POINT('Ctrl Pts',(-194.803373031953,-85.1545718645404,
-10.3812253616273));
#27440=CARTESIAN_POINT('Ctrl Pts',(-194.11814612319,-85.999497126127,-10.1156542867041));
#27441=CARTESIAN_POINT('Ctrl Pts',(-192.738313170377,-87.6603590181507,
-9.52788750796532));
#27442=CARTESIAN_POINT('Ctrl Pts',(-192.043668081395,-88.4763296708027,
-9.20586973247695));
#27443=CARTESIAN_POINT('Ctrl Pts',(-190.649625487509,-90.0758715417795,
-8.48578531610911));
#27444=CARTESIAN_POINT('Ctrl Pts',(-189.950117761389,-90.8595415714283,
-8.0882283586907));
#27445=CARTESIAN_POINT('Ctrl Pts',(-189.252344883447,-91.6237366354615,
-7.63473361656836));
#27446=CARTESIAN_POINT('Origin',(1.35935794705356E-14,222.,0.));
#27447=CARTESIAN_POINT('Origin',(0.,0.,0.));
#27448=CARTESIAN_POINT('',(-3.15824218834415E-14,-222.,15.));
#27449=CARTESIAN_POINT('',(-3.15824218834415E-14,-207.,-1.83697019872103E-15));
#27450=CARTESIAN_POINT('Origin',(-2.77555756156289E-14,-222.,0.));
#27451=CARTESIAN_POINT('Origin',(-2.77555756156289E-14,-222.,0.));
#27452=CARTESIAN_POINT('',(-183.040047979333,-96.6713030620957,1.55769866206538E-14));
#27453=CARTESIAN_POINT('Origin',(0.,0.,-1.83697019872103E-15));
#27454=CARTESIAN_POINT('',(-188.203666712899,91.5667089479117,7.97650136887543));
#27455=CARTESIAN_POINT('Ctrl Pts',(-183.040047979333,-96.6713030620957,
1.55769866197491E-14));
#27456=CARTESIAN_POINT('Ctrl Pts',(-183.040047979333,-96.6713030620956,
0.291148679290596));
#27457=CARTESIAN_POINT('Ctrl Pts',(-183.058980950331,-96.6535943415814,
0.57974868924173));
#27458=CARTESIAN_POINT('Ctrl Pts',(-183.132993285616,-96.5842492219133,
1.15207487751939));
#27459=CARTESIAN_POINT('Ctrl Pts',(-183.188070480362,-96.5326105208468,
1.43412348751035));
#27460=CARTESIAN_POINT('Ctrl Pts',(-183.327967184294,-96.4010948894287,
1.98002353439478));
#27461=CARTESIAN_POINT('Ctrl Pts',(-183.413460182539,-96.3205813016289,
2.24681133290275));
#27462=CARTESIAN_POINT('Ctrl Pts',(-183.608674914206,-96.1360952072225,
2.76184779141642));
#27463=CARTESIAN_POINT('Ctrl Pts',(-183.717592481392,-96.0328819217764,
3.00851618547335));
#27464=CARTESIAN_POINT('Ctrl Pts',(-183.953720315568,-95.8082188834415,
3.4840703792612));
#27465=CARTESIAN_POINT('Ctrl Pts',(-184.080951141305,-95.6867496989865,
3.71293669895085));
#27466=CARTESIAN_POINT('Ctrl Pts',(-184.350664529886,-95.4280873250007,
4.15559630117501));
#27467=CARTESIAN_POINT('Ctrl Pts',(-184.493074751668,-95.2909557075865,
4.36905997833143));
#27468=CARTESIAN_POINT('Ctrl Pts',(-184.931498282134,-94.8667492919688,
4.97954692467032));
#27469=CARTESIAN_POINT('Ctrl Pts',(-185.241141223251,-94.5645177651879,
5.35155104444554));
#27470=CARTESIAN_POINT('Ctrl Pts',(-186.203958736528,-93.6146152438495,
6.39425281757349));
#27471=CARTESIAN_POINT('Ctrl Pts',(-186.891302371369,-92.9233052227938,
6.99367622818273));
#27472=CARTESIAN_POINT('Ctrl Pts',(-188.305681714773,-91.4656918334382,
8.07241329266994));
#27473=CARTESIAN_POINT('Ctrl Pts',(-189.018430897681,-90.7143285017377,
8.53970972029528));
#27474=CARTESIAN_POINT('Ctrl Pts',(-190.442802070271,-89.1760731637858,
9.38285699584151));
#27475=CARTESIAN_POINT('Ctrl Pts',(-191.15461822974,-88.3890133117134,9.7578302902465));
#27476=CARTESIAN_POINT('Ctrl Pts',(-192.571192569202,-86.7836262630972,
10.4408468314537));
#27477=CARTESIAN_POINT('Ctrl Pts',(-193.27601245978,-85.96524723729,10.748615183262));
#27478=CARTESIAN_POINT('Ctrl Pts',(-195.374252691012,-83.4669421359547,
11.5939771576598));
#27479=CARTESIAN_POINT('Ctrl Pts',(-196.751203470348,-81.7440535365057,
12.0547297956035));
#27480=CARTESIAN_POINT('Ctrl Pts',(-198.769971299121,-79.0815725360579,
12.6433844340074));
#27481=CARTESIAN_POINT('Ctrl Pts',(-199.436591021777,-78.1790237365388,
12.8224654289728));
#27482=CARTESIAN_POINT('Ctrl Pts',(-200.744763817792,-76.3598416721392,
13.1491235542598));
#27483=CARTESIAN_POINT('Ctrl Pts',(-201.386303874719,-75.4433717087901,
13.2967666638446));
#27484=CARTESIAN_POINT('Ctrl Pts',(-203.273408069987,-72.6737796512646,
13.7004868908735));
#27485=CARTESIAN_POINT('Ctrl Pts',(-204.481466008945,-70.8004978383475,
13.9177067702817));
#27486=CARTESIAN_POINT('Ctrl Pts',(-207.956458983342,-65.1026091973039,
14.4573854330589));
#27487=CARTESIAN_POINT('Ctrl Pts',(-210.074493786179,-61.2001921411133,
14.6697866179376));
#27488=CARTESIAN_POINT('Ctrl Pts',(-213.912886037181,-53.1943214976126,
14.9353299175372));
#27489=CARTESIAN_POINT('Ctrl Pts',(-215.633323467389,-49.0908222055926,
14.986792054574));
#27490=CARTESIAN_POINT('Ctrl Pts',(-217.908396227818,-42.7841937443938,
15.0032413379716));
#27491=CARTESIAN_POINT('Ctrl Pts',(-218.615742309528,-40.6567017058131,
14.998335228712));
#27492=CARTESIAN_POINT('Ctrl Pts',(-219.926088227278,-36.350417240132,14.9755428583751));
#27493=CARTESIAN_POINT('Ctrl Pts',(-220.529800921946,-34.1674257024326,
14.9575922154785));
#27494=CARTESIAN_POINT('Ctrl Pts',(-222.161510126542,-27.6207361803836,
14.8952029196392));
#27495=CARTESIAN_POINT('Ctrl Pts',(-223.018675922415,-23.2357106926463,
14.8428468498203));
#27496=CARTESIAN_POINT('Ctrl Pts',(-224.286108963103,-14.4256282001768,
14.7563556073774));
#27497=CARTESIAN_POINT('Ctrl Pts',(-224.696337066657,-10.0005680076165,
14.7221538153805));
#27498=CARTESIAN_POINT('Ctrl Pts',(-225.070163176114,-1.11035032097217,
14.6912120318798));
#27499=CARTESIAN_POINT('Ctrl Pts',(-225.033793040228,3.35480449941421,14.6945093265208));
#27500=CARTESIAN_POINT('Ctrl Pts',(-224.700737496435,8.96206207694743,14.721618144576));
#27501=CARTESIAN_POINT('Ctrl Pts',(-224.619710847452,10.0848072650507,14.7281381219928));
#27502=CARTESIAN_POINT('Ctrl Pts',(-224.428465136887,12.3329162515791,14.7431531378288));
#27503=CARTESIAN_POINT('Ctrl Pts',(-224.318164098119,13.458479623482,14.7516532939685));
#27504=CARTESIAN_POINT('Ctrl Pts',(-223.945632319424,16.8171559006165,14.7794486414301));
#27505=CARTESIAN_POINT('Ctrl Pts',(-223.641247849546,19.0396172614184,14.8011160303732));
#27506=CARTESIAN_POINT('Ctrl Pts',(-222.563939303659,25.6581889778629,14.8699597930253));
#27507=CARTESIAN_POINT('Ctrl Pts',(-221.627271804797,30.0056107522321,14.9215038566953));
#27508=CARTESIAN_POINT('Ctrl Pts',(-219.327317476923,38.5734928326465,14.9935819020374));
#27509=CARTESIAN_POINT('Ctrl Pts',(-217.964011313114,42.793947973277,15.0143464053309));
#27510=CARTESIAN_POINT('Ctrl Pts',(-214.807994247347,51.1069121038375,14.9632933929592));
#27511=CARTESIAN_POINT('Ctrl Pts',(-213.015330352922,55.1994371694619,14.8923013616224));
#27512=CARTESIAN_POINT('Ctrl Pts',(-210.496052823544,60.2319818480121,14.6864216598738));
#27513=CARTESIAN_POINT('Ctrl Pts',(-209.977518875153,61.2356634382941,14.6391865829707));
#27514=CARTESIAN_POINT('Ctrl Pts',(-208.915699033734,63.2279335470269,14.530991204538));
#27515=CARTESIAN_POINT('Ctrl Pts',(-208.373138206947,64.2152547465443,14.4701199370589));
#27516=CARTESIAN_POINT('Ctrl Pts',(-206.711108280302,67.1507229882156,14.2641249010502));
#27517=CARTESIAN_POINT('Ctrl Pts',(-205.55728638811,69.0724061150207,14.0958534464656));
#27518=CARTESIAN_POINT('Ctrl Pts',(-203.161251585093,72.8442174373689,13.6766605958867));
#27519=CARTESIAN_POINT('Ctrl Pts',(-201.919013597683,74.6943624357747,13.4259631930999));
#27520=CARTESIAN_POINT('Ctrl Pts',(-199.349782492321,78.3209577812108,12.8114190642419));
#27521=CARTESIAN_POINT('Ctrl Pts',(-198.022727586167,80.0974546194972,12.4481581938624));
#27522=CARTESIAN_POINT('Ctrl Pts',(-195.97252063722,82.7037994050085,11.7799394449392));
#27523=CARTESIAN_POINT('Ctrl Pts',(-195.279197353805,83.562828999768,11.5364478286467));
#27524=CARTESIAN_POINT('Ctrl Pts',(-193.873779899557,85.2604683721014,10.9970720898174));
#27525=CARTESIAN_POINT('Ctrl Pts',(-193.164004359316,86.0961634161304,10.7020151751908));
#27526=CARTESIAN_POINT('Ctrl Pts',(-191.743919945876,87.7276352163228,10.0519934684016));
#27527=CARTESIAN_POINT('Ctrl Pts',(-191.032198859638,88.5251060018795,9.69668774260903));
#27528=CARTESIAN_POINT('Ctrl Pts',(-189.612385303067,90.078853967896,8.9054582820669));
#27529=CARTESIAN_POINT('Ctrl Pts',(-188.904144762275,90.8352574843552,8.47000883192016));
#27530=CARTESIAN_POINT('Ctrl Pts',(-188.203666712899,91.5667089479117,7.97650136887543));
#27531=CARTESIAN_POINT('',(-183.040047979333,96.6713030620956,-1.78040965343628E-11));
#27532=CARTESIAN_POINT('Ctrl Pts',(-188.203666712899,91.5667089479117,7.97650136887544));
#27533=CARTESIAN_POINT('Ctrl Pts',(-188.021076801371,91.7573725356387,7.84786138637183));
#27534=CARTESIAN_POINT('Ctrl Pts',(-187.839014153582,91.9463367031238,7.7152484090642));
#27535=CARTESIAN_POINT('Ctrl Pts',(-187.657688363759,92.1334355047595,7.57806657321992));
#27536=CARTESIAN_POINT('Ctrl Pts',(-187.482614389677,92.3140834466786,7.44561454200802));
#27537=CARTESIAN_POINT('Ctrl Pts',(-187.308227372814,92.4929924341846,7.30890311629443));
#27538=CARTESIAN_POINT('Ctrl Pts',(-187.134710929371,92.6700205956967,7.16744440176363));
#27539=CARTESIAN_POINT('Ctrl Pts',(-187.108293925377,92.6969722410681,7.14590802542574));
#27540=CARTESIAN_POINT('Ctrl Pts',(-187.081897089628,92.7238803062719,7.1242617107976));
#27541=CARTESIAN_POINT('Ctrl Pts',(-187.055521058621,92.7507443066074,7.10250384250346));
#27542=CARTESIAN_POINT('Ctrl Pts',(-186.902111764284,92.9069917470796,6.97595488521369));
#27543=CARTESIAN_POINT('Ctrl Pts',(-186.749275961903,93.0618767690438,6.84556443583174));
#27544=CARTESIAN_POINT('Ctrl Pts',(-186.597357972257,93.2150934975638,6.71079465634692));
#27545=CARTESIAN_POINT('Ctrl Pts',(-186.562877573727,93.2498686672017,6.68020633881195));
#27546=CARTESIAN_POINT('Ctrl Pts',(-186.528444397317,93.2845579577452,6.64939261767227));
#27547=CARTESIAN_POINT('Ctrl Pts',(-186.494062363408,93.3191579039876,6.61834755243621));
#27548=CARTESIAN_POINT('Ctrl Pts',(-186.387663841254,93.4262307768882,6.52227560189259));
#27549=CARTESIAN_POINT('Ctrl Pts',(-186.281628729357,93.5325860908707,6.42388081224351));
#27550=CARTESIAN_POINT('Ctrl Pts',(-186.176231882927,93.6379436507861,6.32312127204413));
#27551=CARTESIAN_POINT('Ctrl Pts',(-186.088224400876,93.7259183281816,6.23898598976658));
#27552=CARTESIAN_POINT('Ctrl Pts',(-186.000661983538,93.8131974648858,6.15320249997137));
#27553=CARTESIAN_POINT('Ctrl Pts',(-185.913702242406,93.8996252320157,6.06577333665428));
#27554=CARTESIAN_POINT('Ctrl Pts',(-185.830659834658,93.98215962995,5.98228265309385));
#27555=CARTESIAN_POINT('Ctrl Pts',(-185.748282632558,94.0638023049231,5.89745987433741));
#27556=CARTESIAN_POINT('Ctrl Pts',(-185.666724552854,94.1444112466403,5.81120124899772));
#27557=CARTESIAN_POINT('Ctrl Pts',(-185.565754072301,94.2442066760027,5.70441140200803));
#27558=CARTESIAN_POINT('Ctrl Pts',(-185.465966572545,94.3425454523725,5.59540453025664));
#27559=CARTESIAN_POINT('Ctrl Pts',(-185.36752368835,94.4392774100917,5.4838933269904));
#27560=CARTESIAN_POINT('Ctrl Pts',(-185.271466218412,94.5336654117913,5.37508420235797));
#27561=CARTESIAN_POINT('Ctrl Pts',(-185.176689032625,94.6265235208791,5.26389056210744));
#27562=CARTESIAN_POINT('Ctrl Pts',(-185.083333271035,94.7177251966252,5.15009214619747));
#27563=CARTESIAN_POINT('Ctrl Pts',(-185.017242203712,94.7822912822002,5.06952873330148));
#27564=CARTESIAN_POINT('Ctrl Pts',(-184.95186335678,94.8460274452087,4.98766078741659));
#27565=CARTESIAN_POINT('Ctrl Pts',(-184.88724379259,94.9088928760068,4.9044251869639));
#27566=CARTESIAN_POINT('Ctrl Pts',(-184.860768537757,94.9346494455754,4.87032276363793));
#27567=CARTESIAN_POINT('Ctrl Pts',(-184.834419684901,94.9602607323629,4.83598937607995));
#27568=CARTESIAN_POINT('Ctrl Pts',(-184.80820176871,94.9857229573254,4.80142347587037));
#27569=CARTESIAN_POINT('Ctrl Pts',(-184.732754718691,95.0589953618257,4.70195351101801));
#27570=CARTESIAN_POINT('Ctrl Pts',(-184.658322875617,95.1310996942388,4.60036233156195));
#27571=CARTESIAN_POINT('Ctrl Pts',(-184.585276389778,95.2016996031477,4.49675562307688));
#27572=CARTESIAN_POINT('Ctrl Pts',(-184.514231589108,95.2703648701778,4.39598803832812));
#27573=CARTESIAN_POINT('Ctrl Pts',(-184.444497389723,95.3376069258162,4.29331394586699));
#27574=CARTESIAN_POINT('Ctrl Pts',(-184.376383333509,95.4031461308148,4.18885474060621));
#27575=CARTESIAN_POINT('Ctrl Pts',(-184.345867348177,95.4325085492294,4.14205565459065));
#27576=CARTESIAN_POINT('Ctrl Pts',(-184.315676117797,95.4615295939936,4.09489859062733));
#27577=CARTESIAN_POINT('Ctrl Pts',(-184.285835279432,95.4901862208126,4.04739604433558));
#27578=CARTESIAN_POINT('Ctrl Pts',(-184.250347078743,95.5242660985678,3.9909036671654));
#27579=CARTESIAN_POINT('Ctrl Pts',(-184.215332259082,95.5578521322308,3.93391060486237));
#27580=CARTESIAN_POINT('Ctrl Pts',(-184.180823297309,95.5909168803663,3.87638066206044));
#27581=CARTESIAN_POINT('Ctrl Pts',(-184.122135163681,95.6471488924924,3.77854158498635));
#27582=CARTESIAN_POINT('Ctrl Pts',(-184.06492944055,95.7018658475249,3.67919720543105));
#27583=CARTESIAN_POINT('Ctrl Pts',(-184.009332974402,95.7549582674443,3.57817784229945));
#27584=CARTESIAN_POINT('Ctrl Pts',(-183.954092701837,95.80771053662,3.47780568665149));
#27585=CARTESIAN_POINT('Ctrl Pts',(-183.900441148331,95.8588590170415,3.37577991412729));
#27586=CARTESIAN_POINT('Ctrl Pts',(-183.848484126247,95.908314252787,3.27197868131283));
#27587=CARTESIAN_POINT('Ctrl Pts',(-183.834151916205,95.921956351544,3.24334537994841));
#27588=CARTESIAN_POINT('Ctrl Pts',(-183.819948535722,95.9354697139894,3.21457724453099));
#27589=CARTESIAN_POINT('Ctrl Pts',(-183.805875952186,95.9488527047503,3.18567232341047));
#27590=CARTESIAN_POINT('Ctrl Pts',(-183.760917696567,95.9916078902521,3.09332859497882));
#27591=CARTESIAN_POINT('Ctrl Pts',(-183.717166718273,96.0331520763448,2.99925051740835));
#27592=CARTESIAN_POINT('Ctrl Pts',(-183.674920024759,96.0732153826263,2.90364281121743));
#27593=CARTESIAN_POINT('Ctrl Pts',(-183.647332236574,96.0993773829103,2.84120940098035));
#27594=CARTESIAN_POINT('Ctrl Pts',(-183.620385155488,96.1249086081634,2.77812375522392));
#27595=CARTESIAN_POINT('Ctrl Pts',(-183.594152714823,96.1497420997336,2.71444332769558));
#27596=CARTESIAN_POINT('Ctrl Pts',(-183.552513710988,96.1891605382974,2.61336277632992));
#27597=CARTESIAN_POINT('Ctrl Pts',(-183.512667688487,96.2268302669331,2.5107665238383));
#27598=CARTESIAN_POINT('Ctrl Pts',(-183.474859837213,96.262532942592,2.40684095748967));
#27599=CARTESIAN_POINT('Ctrl Pts',(-183.446737682174,96.2890892304089,2.32953926509386));
#27600=CARTESIAN_POINT('Ctrl Pts',(-183.419742343131,96.3145579714235,2.25150195220109));
#27601=CARTESIAN_POINT('Ctrl Pts',(-183.393961050788,96.3388617174235,2.17280303683206));
#27602=CARTESIAN_POINT('Ctrl Pts',(-183.359580666358,96.3712717347123,2.06785488572363));
#27603=CARTESIAN_POINT('Ctrl Pts',(-183.327343569224,96.4016267776895,1.96172200413313));
#27604=CARTESIAN_POINT('Ctrl Pts',(-183.297389795937,96.4298084395749,1.8542397954829));
#27605=CARTESIAN_POINT('Ctrl Pts',(-183.274245858352,96.4515831461358,1.77119311202647));
#27606=CARTESIAN_POINT('Ctrl Pts',(-183.252464429557,96.4720609088697,1.68734163313003));
#27607=CARTESIAN_POINT('Ctrl Pts',(-183.232098245116,96.4911976665063,1.60262357057942));
#27608=CARTESIAN_POINT('Ctrl Pts',(-183.216389907906,96.5059577529103,1.53728094843953));
#27609=CARTESIAN_POINT('Ctrl Pts',(-183.201534766402,96.5199094694207,1.47135146558728));
#27610=CARTESIAN_POINT('Ctrl Pts',(-183.187602228551,96.5329901074898,1.40511236999388));
#27611=CARTESIAN_POINT('Ctrl Pts',(-183.168469031447,96.5509534124586,1.31414791789888));
#27612=CARTESIAN_POINT('Ctrl Pts',(-183.151038568884,96.5673071210697,1.22241879048284));
#27613=CARTESIAN_POINT('Ctrl Pts',(-183.135478803873,96.5818992004815,1.13048589166228));
#27614=CARTESIAN_POINT('Ctrl Pts',(-183.127438973994,96.5894390210347,1.08298357616052));
#27615=CARTESIAN_POINT('Ctrl Pts',(-183.119898495986,96.5965085951852,1.03542593039518));
#27616=CARTESIAN_POINT('Ctrl Pts',(-183.112880159761,96.6030872601668,0.987885042250572));
#27617=CARTESIAN_POINT('Ctrl Pts',(-183.094272288311,96.6205294214393,0.861838824608398));
#27618=CARTESIAN_POINT('Ctrl Pts',(-183.079158190004,96.6346871142076,0.735294438806359));
#27619=CARTESIAN_POINT('Ctrl Pts',(-183.067609370826,96.6455017519546,0.607979113572891));
#27620=CARTESIAN_POINT('Ctrl Pts',(-183.059751403966,96.6528601722144,0.521352109460987));
#27621=CARTESIAN_POINT('Ctrl Pts',(-183.053544641283,96.6586702885726,0.434367916619133));
#27622=CARTESIAN_POINT('Ctrl Pts',(-183.049021241499,96.6629044452172,0.346936379531023));
#27623=CARTESIAN_POINT('Ctrl Pts',(-183.043938087641,96.6676625631615,0.24868551154289));
#27624=CARTESIAN_POINT('Ctrl Pts',(-183.041042521995,96.6703728479844,0.149377453584831));
#27625=CARTESIAN_POINT('Ctrl Pts',(-183.040310525973,96.6710579738602,0.0500714675686074));
#27626=CARTESIAN_POINT('Ctrl Pts',(-183.040187486682,96.6711731348712,0.0333793849144663));
#27627=CARTESIAN_POINT('Ctrl Pts',(-183.040125617894,96.6712310386364,0.0166872567960485));
#27628=CARTESIAN_POINT('Ctrl Pts',(-183.040124856982,96.67123174467,-7.3835382252696E-10));
#27629=CARTESIAN_POINT('',(6.58230156589418E-15,207.,-1.83697019872103E-15));
#27630=CARTESIAN_POINT('Origin',(0.,0.,-1.83697019872103E-15));
#27631=CARTESIAN_POINT('',(0.,222.,-15.));
#27632=CARTESIAN_POINT('Origin',(0.,222.,0.));
#27633=CARTESIAN_POINT('Origin',(0.,222.,0.));
#27634=CARTESIAN_POINT('',(-188.497895047951,-91.2584808544846,-8.18007173203753));
#27635=CARTESIAN_POINT('Ctrl Pts',(-183.040047979333,96.6713030620956,-1.78040965343625E-11));
#27636=CARTESIAN_POINT('Ctrl Pts',(-183.040047979334,96.671303062095,-0.290717296796128));
#27637=CARTESIAN_POINT('Ctrl Pts',(-183.058923419162,96.6536479752409,-0.578335867620054));
#27638=CARTESIAN_POINT('Ctrl Pts',(-183.132297130496,96.5849017443526,-1.14764968196531));
#27639=CARTESIAN_POINT('Ctrl Pts',(-183.187136433235,96.5334867370368,-1.42960539277542));
#27640=CARTESIAN_POINT('Ctrl Pts',(-183.395676877553,96.3374453080213,-2.24595901383476));
#27641=CARTESIAN_POINT('Ctrl Pts',(-183.596179288576,96.148378129504,-2.76253014436806));
#27642=CARTESIAN_POINT('Ctrl Pts',(-183.948385873179,95.813304980467,-3.47403718087876));
#27643=CARTESIAN_POINT('Ctrl Pts',(-184.074723247574,95.6927020889136,-3.70196303508026));
#27644=CARTESIAN_POINT('Ctrl Pts',(-184.342135655567,95.4362859797969,-4.14231049014845));
#27645=CARTESIAN_POINT('Ctrl Pts',(-184.483878266456,95.2998256542781,-4.35559560516305));
#27646=CARTESIAN_POINT('Ctrl Pts',(-184.922137729314,94.8758603284929,-4.96776945688272));
#27647=CARTESIAN_POINT('Ctrl Pts',(-185.231024285832,94.5744209337779,-5.3396847793381));
#27648=CARTESIAN_POINT('Ctrl Pts',(-186.189742337321,93.6287929397982,-6.38062863151832));
#27649=CARTESIAN_POINT('Ctrl Pts',(-186.870931608401,92.9438803352724,-6.97616626868284));
#27650=CARTESIAN_POINT('Ctrl Pts',(-187.922915121028,91.8603562891812,-7.7814123143153));
#27651=CARTESIAN_POINT('Ctrl Pts',(-188.27976116909,91.4886432157324,-8.03501547234262));
#27652=CARTESIAN_POINT('Ctrl Pts',(-188.991709907376,90.7381517492508,-8.51093004128364));
#27653=CARTESIAN_POINT('Ctrl Pts',(-189.347946938551,90.3582289492531,-8.73415029064059));
#27654=CARTESIAN_POINT('Ctrl Pts',(-190.415704618364,89.2057861435712,-9.36797876968955));
#27655=CARTESIAN_POINT('Ctrl Pts',(-191.126187452397,88.4206612756743,-9.74317222706952));
#27656=CARTESIAN_POINT('Ctrl Pts',(-192.538651519066,86.8210527672942,-10.4260665657394));
#27657=CARTESIAN_POINT('Ctrl Pts',(-193.240691367808,86.0065197832478,-10.7334743463981));
#27658=CARTESIAN_POINT('Ctrl Pts',(-195.328969811832,83.522361710867,-11.5774799750461));
#27659=CARTESIAN_POINT('Ctrl Pts',(-196.697140045752,81.8123666295429,-12.0369899115148));
#27660=CARTESIAN_POINT('Ctrl Pts',(-198.701009621295,79.1739133145013,-12.6241943015858));
#27661=CARTESIAN_POINT('Ctrl Pts',(-199.360982676768,78.2821187303764,-12.8025189004934));
#27662=CARTESIAN_POINT('Ctrl Pts',(-200.663565069239,76.4745743432818,-13.1297934395841));
#27663=CARTESIAN_POINT('Ctrl Pts',(-201.307303606054,75.5571516619106,-13.2789601805961));
#27664=CARTESIAN_POINT('Ctrl Pts',(-203.201516047313,72.7832478647282,-13.6867621695905));
#27665=CARTESIAN_POINT('Ctrl Pts',(-204.413700546118,70.9075282912295,-13.9060360996326));
#27666=CARTESIAN_POINT('Ctrl Pts',(-207.899657365585,65.2035836701327,-14.4507645550931));
#27667=CARTESIAN_POINT('Ctrl Pts',(-210.023128099383,61.2987994893877,-14.6650896802637));
#27668=CARTESIAN_POINT('Ctrl Pts',(-213.870276136955,53.2915163853001,-14.933497953333));
#27669=CARTESIAN_POINT('Ctrl Pts',(-215.594021132889,49.1889740960755,-14.985853687648));
#27670=CARTESIAN_POINT('Ctrl Pts',(-217.873399431556,42.8864129541246,-15.0033037809541));
#27671=CARTESIAN_POINT('Ctrl Pts',(-218.582069674932,40.7607166635472,-14.9986689688532));
#27672=CARTESIAN_POINT('Ctrl Pts',(-219.56675968207,37.5343872263211,-14.9819099628708));
#27673=CARTESIAN_POINT('Ctrl Pts',(-219.8822170261,36.4514838658265,-14.9746676310821));
#27674=CARTESIAN_POINT('Ctrl Pts',(-220.483358450152,34.2853764016843,-14.9578746973126));
#27675=CARTESIAN_POINT('Ctrl Pts',(-220.769465484776,33.2008912844799,-14.9483204745317));
#27676=CARTESIAN_POINT('Ctrl Pts',(-222.12855866699,27.7713853384315,-14.8968645760071));
#27677=CARTESIAN_POINT('Ctrl Pts',(-222.987787020107,23.4051756849622,-14.8447490296456));
#27678=CARTESIAN_POINT('Ctrl Pts',(-224.263142252711,14.6286399575493,-14.7581200953001));
#27679=CARTESIAN_POINT('Ctrl Pts',(-224.67923658837,10.2183109541443,-14.7235458426584));
#27680=CARTESIAN_POINT('Ctrl Pts',(-225.067487120359,1.35335614042816,-14.6914557569397));
#27681=CARTESIAN_POINT('Ctrl Pts',(-225.039680369902,-3.10126619891411,
-14.6939820956571));
#27682=CARTESIAN_POINT('Ctrl Pts',(-224.65412178184,-9.81750421703877,-14.7254343338351));
#27683=CARTESIAN_POINT('Ctrl Pts',(-224.4672482405,-12.0685257533435,-14.740436703992));
#27684=CARTESIAN_POINT('Ctrl Pts',(-223.981935807087,-16.5303006920475,
-14.7768220386414));
#27685=CARTESIAN_POINT('Ctrl Pts',(-223.683613303296,-18.7451256741302,
-14.7981937237368));
#27686=CARTESIAN_POINT('Ctrl Pts',(-222.625392381006,-25.3424864211294,
-14.8664210701889));
#27687=CARTESIAN_POINT('Ctrl Pts',(-221.702647102239,-29.6780260824246,
-14.9179126495301));
#27688=CARTESIAN_POINT('Ctrl Pts',(-219.432103438233,-38.226379286061,-14.9914332557902));
#27689=CARTESIAN_POINT('Ctrl Pts',(-218.084289955228,-42.4391887915816,
-15.0136856420233));
#27690=CARTESIAN_POINT('Ctrl Pts',(-214.960123702443,-50.7409884267741,
-14.9681429282199));
#27691=CARTESIAN_POINT('Ctrl Pts',(-213.183822160821,-54.8299944921915,
-14.9011481177155));
#27692=CARTESIAN_POINT('Ctrl Pts',(-210.685097784923,-59.8607475849498,
-14.702829183641));
#27693=CARTESIAN_POINT('Ctrl Pts',(-210.170653953151,-60.8642286915694,
-14.6572311370428));
#27694=CARTESIAN_POINT('Ctrl Pts',(-209.118711926601,-62.8532204215151,
-14.5527940286245));
#27695=CARTESIAN_POINT('Ctrl Pts',(-208.580972841412,-63.8393132496125,
-14.4939525317814));
#27696=CARTESIAN_POINT('Ctrl Pts',(-206.932956196544,-66.7723267156479,
-14.2945370605171));
#27697=CARTESIAN_POINT('Ctrl Pts',(-205.78787826466,-68.6940106709314,-14.1313021234452));
#27698=CARTESIAN_POINT('Ctrl Pts',(-203.40751840668,-72.4691497536957,-13.7237471362256));
#27699=CARTESIAN_POINT('Ctrl Pts',(-202.172215713411,-74.3226190289864,
-13.4796454873293));
#27700=CARTESIAN_POINT('Ctrl Pts',(-199.614242706283,-77.9593665780488,
-12.880290719481));
#27701=CARTESIAN_POINT('Ctrl Pts',(-198.291521481218,-79.7426835304235,
-12.5256047378343));
#27702=CARTESIAN_POINT('Ctrl Pts',(-196.24496263622,-82.3622188310058,-11.872433441665));
#27703=CARTESIAN_POINT('Ctrl Pts',(-195.553967137143,-83.2240348135499,
-11.6347489559485));
#27704=CARTESIAN_POINT('Ctrl Pts',(-194.162346915831,-84.9164771058137,
-11.1125529770436));
#27705=CARTESIAN_POINT('Ctrl Pts',(-193.460866402951,-85.7481952744176,
-10.8278555945698));
#27706=CARTESIAN_POINT('Ctrl Pts',(-192.050013622452,-87.3804628822538,
-10.1985906850403));
#27707=CARTESIAN_POINT('Ctrl Pts',(-191.340598963084,-88.1810474344335,
-9.85419988852607));
#27708=CARTESIAN_POINT('Ctrl Pts',(-189.919091050928,-89.7474499656185,
-9.08558654970619));
#27709=CARTESIAN_POINT('Ctrl Pts',(-189.206880667753,-90.5133679110211,
-8.66185957465181));
#27710=CARTESIAN_POINT('Ctrl Pts',(-188.497895047951,-91.2584808544846,
-8.18007173203753));
#27711=CARTESIAN_POINT('Ctrl Pts',(-188.497895047951,-91.2584808544846,
-8.18007173203754));
#27712=CARTESIAN_POINT('Ctrl Pts',(-188.300062055738,-91.4663946950838,
-8.0456352528558));
#27713=CARTESIAN_POINT('Ctrl Pts',(-188.103136583577,-91.6719902155658,
-7.90706781866979));
#27714=CARTESIAN_POINT('Ctrl Pts',(-187.907384188659,-91.8750715954411,
-7.76381635884333));
#27715=CARTESIAN_POINT('Ctrl Pts',(-187.718661179823,-92.0708604084685,
-7.6257089986259));
#27716=CARTESIAN_POINT('Ctrl Pts',(-187.531028538814,-92.2643124052881,
-7.48324791185683));
#27717=CARTESIAN_POINT('Ctrl Pts',(-187.344714547772,-92.455262437099,-7.33598118338943));
#27718=CARTESIAN_POINT('Ctrl Pts',(-187.176146527014,-92.6280249266267,
-7.20274126510646));
#27719=CARTESIAN_POINT('Ctrl Pts',(-187.008650204035,-92.7987460149388,
-7.0656087741307));
#27720=CARTESIAN_POINT('Ctrl Pts',(-186.842467463592,-92.9672410175639,
-6.92394517460035));
#27721=CARTESIAN_POINT('Ctrl Pts',(-186.799612610027,-93.0106921524095,
-6.88741326522613));
#27722=CARTESIAN_POINT('Ctrl Pts',(-186.75684505207,-93.0539953071172,-6.85058028783488));
#27723=CARTESIAN_POINT('Ctrl Pts',(-186.714168812212,-93.0971474350744,
-6.81343583506232));
#27724=CARTESIAN_POINT('Ctrl Pts',(-186.568967960517,-93.2439674396628,
-6.68705623376176));
#27725=CARTESIAN_POINT('Ctrl Pts',(-186.424842134083,-93.3890455019234,
-6.55710606451584));
#27726=CARTESIAN_POINT('Ctrl Pts',(-186.281951647043,-93.5322032134759,
-6.42315381606293));
#27727=CARTESIAN_POINT('Ctrl Pts',(-186.257009039101,-93.5571924674637,
-6.3997714448129));
#27728=CARTESIAN_POINT('Ctrl Pts',(-186.231992582235,-93.582233475522,-6.3761612335205));
#27729=CARTESIAN_POINT('Ctrl Pts',(-186.206930421579,-93.6072983045629,
-6.35234366750294));
#27730=CARTESIAN_POINT('Ctrl Pts',(-186.144618582895,-93.6696167776295,
-6.29312625397292));
#27731=CARTESIAN_POINT('Ctrl Pts',(-186.082020331053,-93.73208556107,-6.23264317803972));
#27732=CARTESIAN_POINT('Ctrl Pts',(-186.019574250509,-93.7942745571904,
-6.17119264600906));
#27733=CARTESIAN_POINT('Ctrl Pts',(-185.963251794942,-93.8503651387019,
-6.1157681128792));
#27734=CARTESIAN_POINT('Ctrl Pts',(-185.907053155763,-93.9062281788253,
-6.05955663501713));
#27735=CARTESIAN_POINT('Ctrl Pts',(-185.851294277388,-93.961557772832,-6.00281180135348));
#27736=CARTESIAN_POINT('Ctrl Pts',(-185.749818148972,-94.0622526424254,
-5.8995413232585));
#27737=CARTESIAN_POINT('Ctrl Pts',(-185.64944798569,-94.1615675588845,-5.79419527240436));
#27738=CARTESIAN_POINT('Ctrl Pts',(-185.550310946567,-94.2593715002356,
-5.68653596243487));
#27739=CARTESIAN_POINT('Ctrl Pts',(-185.453240346919,-94.3551367895654,
-5.58112073247738));
#27740=CARTESIAN_POINT('Ctrl Pts',(-185.357352047033,-94.4494534467525,
-5.473487596431));
#27741=CARTESIAN_POINT('Ctrl Pts',(-185.262760907272,-94.5422101471869,
-5.36346162345762));
#27742=CARTESIAN_POINT('Ctrl Pts',(-185.207680102582,-94.5962227504107,
-5.29939305272703));
#27743=CARTESIAN_POINT('Ctrl Pts',(-185.153039048079,-94.649706625106,-5.23451403425678));
#27744=CARTESIAN_POINT('Ctrl Pts',(-185.098859601402,-94.7026416531689,
-5.16879796046587));
#27745=CARTESIAN_POINT('Ctrl Pts',(-185.074330592064,-94.7266072688649,
-5.13904589973869));
#27746=CARTESIAN_POINT('Ctrl Pts',(-185.049896921581,-94.7504597611539,
-5.10911917048002));
#27747=CARTESIAN_POINT('Ctrl Pts',(-185.025562001606,-94.7741960738258,
-5.07900945369665));
#27748=CARTESIAN_POINT('Ctrl Pts',(-184.946413429458,-94.8513976942973,
-4.98107853410751));
#27749=CARTESIAN_POINT('Ctrl Pts',(-184.868310362198,-94.9273894652854,
-4.88123324740708));
#27750=CARTESIAN_POINT('Ctrl Pts',(-184.791382991276,-95.002060866969,-4.77925814868048));
#27751=CARTESIAN_POINT('Ctrl Pts',(-184.714455620355,-95.0767322686525,
-4.67728304995388));
#27752=CARTESIAN_POINT('Ctrl Pts',(-184.638704007293,-95.1500832519385,
-4.57317788266935));
#27753=CARTESIAN_POINT('Ctrl Pts',(-184.564246641858,-95.2220151025974,
-4.46678202474539));
#27754=CARTESIAN_POINT('Ctrl Pts',(-184.497056056092,-95.2869266550372,
-4.37077003217547));
#27755=CARTESIAN_POINT('Ctrl Pts',(-184.430943906992,-95.3506568984757,
-4.2729026001225));
#27756=CARTESIAN_POINT('Ctrl Pts',(-184.366226272981,-95.412919659581,-4.17327681029906));
#27757=CARTESIAN_POINT('Ctrl Pts',(-184.334563669764,-95.4433812351646,
-4.12453566112887));
#27758=CARTESIAN_POINT('Ctrl Pts',(-184.303234341527,-95.4734920445134,
-4.07537395381293));
#27759=CARTESIAN_POINT('Ctrl Pts',(-184.272272264877,-95.5032214550723,
-4.0258048980475));
#27760=CARTESIAN_POINT('Ctrl Pts',(-184.206611201955,-95.5662684114961,
-3.92068414253747));
#27761=CARTESIAN_POINT('Ctrl Pts',(-184.142567466176,-95.6276314764618,
-3.81366921333017));
#27762=CARTESIAN_POINT('Ctrl Pts',(-184.080412946787,-95.6870699231794,
-3.70484958990335));
#27763=CARTESIAN_POINT('Ctrl Pts',(-184.072028903129,-95.6950875948971,
-3.69017087494246));
#27764=CARTESIAN_POINT('Ctrl Pts',(-184.063679179314,-95.7030702979177,
-3.67545934343523));
#27765=CARTESIAN_POINT('Ctrl Pts',(-184.055364391027,-95.71101748865,-3.66071523418955));
#27766=CARTESIAN_POINT('Ctrl Pts',(-183.999462471019,-95.7644479796339,
-3.56158775346746));
#27767=CARTESIAN_POINT('Ctrl Pts',(-183.944910782877,-95.8164915916668,
-3.46059627411805));
#27768=CARTESIAN_POINT('Ctrl Pts',(-183.892007949902,-95.8668829533374,
-3.35779889575907));
#27769=CARTESIAN_POINT('Ctrl Pts',(-183.83899400497,-95.9173801521151,-3.25478561180084));
#27770=CARTESIAN_POINT('Ctrl Pts',(-183.787635848404,-95.9662181505276,
-3.14995885084012));
#27771=CARTESIAN_POINT('Ctrl Pts',(-183.738196574503,-96.0131639139981,
-3.04339088491695));
#27772=CARTESIAN_POINT('Ctrl Pts',(-183.70441834109,-96.0452385144339,-2.97058080209866));
#27773=CARTESIAN_POINT('Ctrl Pts',(-183.671535061622,-96.0764305291934,
-2.8969582139391));
#27774=CARTESIAN_POINT('Ctrl Pts',(-183.639620656277,-96.106674727365,-2.82254979915783));
#27775=CARTESIAN_POINT('Ctrl Pts',(-183.625882932619,-96.1196935015595,
-2.79052030560972));
#27776=CARTESIAN_POINT('Ctrl Pts',(-183.612325271825,-96.1325356385398,
-2.75834550238426));
#27777=CARTESIAN_POINT('Ctrl Pts',(-183.598953725412,-96.1451958361621,
-2.72602941545094));
#27778=CARTESIAN_POINT('Ctrl Pts',(-183.559671567108,-96.1823882349924,
-2.63109307798464));
#27779=CARTESIAN_POINT('Ctrl Pts',(-183.522065131717,-96.2179455935306,
-2.5352045733376));
#27780=CARTESIAN_POINT('Ctrl Pts',(-183.486282382413,-96.2517422824135,
-2.43826741633881));
#27781=CARTESIAN_POINT('Ctrl Pts',(-183.4507080064,-96.2853421634085,-2.34189475242377));
#27782=CARTESIAN_POINT('Ctrl Pts',(-183.416936172958,-96.3172017871073,
-2.24448556910026));
#27783=CARTESIAN_POINT('Ctrl Pts',(-183.385084418382,-96.3472227051745,
-2.14598002821041));
#27784=CARTESIAN_POINT('Ctrl Pts',(-183.353419282572,-96.3770677313077,
-2.04805162923407));
#27785=CARTESIAN_POINT('Ctrl Pts',(-183.323651806033,-96.4050955186365,
-1.94903966326626));
#27786=CARTESIAN_POINT('Ctrl Pts',(-183.295869501762,-96.4312344867279,
-1.84892047240775));
#27787=CARTESIAN_POINT('Ctrl Pts',(-183.276527910854,-96.4494320135649,
-1.77921911096964));
#27788=CARTESIAN_POINT('Ctrl Pts',(-183.258147894583,-96.4667146064943,
-1.70898184056822));
#27789=CARTESIAN_POINT('Ctrl Pts',(-183.240750872462,-96.4830654179867,
-1.6382108706281));
#27790=CARTESIAN_POINT('Ctrl Pts',(-183.227158803033,-96.4958400965205,
-1.58291842285402));
#27791=CARTESIAN_POINT('Ctrl Pts',(-183.214149487226,-96.5080622644032,
-1.52710078869208));
#27792=CARTESIAN_POINT('Ctrl Pts',(-183.201778674498,-96.5196811723908,
-1.47094697429921));
#27793=CARTESIAN_POINT('Ctrl Pts',(-183.182833430955,-96.537474913706,-1.38495038595907));
#27794=CARTESIAN_POINT('Ctrl Pts',(-183.165335520778,-96.5538973659424,
-1.29792703960836));
#27795=CARTESIAN_POINT('Ctrl Pts',(-183.149458653825,-96.5687909504186,
-1.21032489975144));
#27796=CARTESIAN_POINT('Ctrl Pts',(-183.138155472576,-96.5793941056436,
-1.1479585104899));
#27797=CARTESIAN_POINT('Ctrl Pts',(-183.12767372067,-96.5892225243258,-1.08529737450488));
#27798=CARTESIAN_POINT('Ctrl Pts',(-183.118075583124,-96.5982196502656,
-1.02248733130099));
#27799=CARTESIAN_POINT('Ctrl Pts',(-183.103912230031,-96.6114961292588,
-0.929802597894992));
#27800=CARTESIAN_POINT('Ctrl Pts',(-183.091641950435,-96.6229920891114,
-0.836874057660911));
#27801=CARTESIAN_POINT('Ctrl Pts',(-183.081282937533,-96.6326945944338,
-0.743544356439005));
#27802=CARTESIAN_POINT('Ctrl Pts',(-183.069236032265,-96.6439780211072,
-0.635007560508499));
#27803=CARTESIAN_POINT('Ctrl Pts',(-183.059794785879,-96.6528172613218,
-0.526131955687998));
#27804=CARTESIAN_POINT('Ctrl Pts',(-183.05299282205,-96.6591851125678,-0.416662911030544));
#27805=CARTESIAN_POINT('Ctrl Pts',(-183.052127587993,-96.6599951259555,
-0.402738058159433));
#27806=CARTESIAN_POINT('Ctrl Pts',(-183.051305108022,-96.660765104651,-0.388803583785994));
#27807=CARTESIAN_POINT('Ctrl Pts',(-183.050525494592,-96.6614949518932,
-0.374858946693551));
#27808=CARTESIAN_POINT('Ctrl Pts',(-183.045113804408,-96.6665611898578,
-0.278062184637631));
#27809=CARTESIAN_POINT('Ctrl Pts',(-183.041826513527,-96.669638755822,-0.180534200127789));
#27810=CARTESIAN_POINT('Ctrl Pts',(-183.040628942412,-96.6707598747363,
-0.0830679383035017));
#27811=CARTESIAN_POINT('Ctrl Pts',(-183.040288591815,-96.6710784975613,
-0.0553679545761854));
#27812=CARTESIAN_POINT('Ctrl Pts',(-183.040117202872,-96.6712389343265,
-0.0276727228799533));
#27813=CARTESIAN_POINT('Ctrl Pts',(-183.04011439547,-96.6712415351879,1.37667022226395E-9));
#27814=CARTESIAN_POINT('Ctrl Pts',(-188.957144201311,90.8303388274957,5.37500533271896));
#27815=CARTESIAN_POINT('Ctrl Pts',(-188.724920768398,91.1301703614817,6.55330325436076));
#27816=CARTESIAN_POINT('Ctrl Pts',(-189.086176933001,91.8055258010517,7.52572239671998));
#27817=CARTESIAN_POINT('Ctrl Pts',(-188.593855532332,91.2997460800671,5.17875473137162));
#27818=CARTESIAN_POINT('Ctrl Pts',(-188.358392135328,91.6013100563716,6.30706395511774));
#27819=CARTESIAN_POINT('Ctrl Pts',(-188.672178961879,92.2572808761228,7.25093082992469));
#27820=CARTESIAN_POINT('Ctrl Pts',(-188.230166171018,91.7638380268742,4.96746400526744));
#27821=CARTESIAN_POINT('Ctrl Pts',(-187.990226260873,92.0686730594487,6.04280873676479));
#27822=CARTESIAN_POINT('Ctrl Pts',(-188.25791121472,92.7031848330253,6.95510627280203));
#27823=CARTESIAN_POINT('Ctrl Pts',(-187.539693143008,92.6343805277346,4.52454205690639));
#27824=CARTESIAN_POINT('Ctrl Pts',(-187.291011725483,92.9455045001231,5.49198587002716));
#27825=CARTESIAN_POINT('Ctrl Pts',(-187.471668401951,93.5383530782691,6.3349561219722));
#27826=CARTESIAN_POINT('Ctrl Pts',(-187.212048839638,93.0429197330079,4.29662107665932));
#27827=CARTESIAN_POINT('Ctrl Pts',(-186.959279127768,93.3569115666992,5.21014878574447));
#27828=CARTESIAN_POINT('Ctrl Pts',(-187.098702415434,93.9297277637807,6.01583633368207));
#27829=CARTESIAN_POINT('Ctrl Pts',(-186.564202659971,93.8422554296375,3.7905424310452));
#27830=CARTESIAN_POINT('Ctrl Pts',(-186.303378595483,94.1617059643359,4.58745384323657));
#27831=CARTESIAN_POINT('Ctrl Pts',(-186.361481988203,94.6944082162028,5.30725885908418));
#27832=CARTESIAN_POINT('Ctrl Pts',(-186.246046490499,94.2305182540288,3.51471556151069));
#27833=CARTESIAN_POINT('Ctrl Pts',(-185.981150185696,94.552750507534,4.24970897101787));
#27834=CARTESIAN_POINT('Ctrl Pts',(-185.999555835803,95.0652888521504,4.92106466935472));
#27835=CARTESIAN_POINT('Ctrl Pts',(-185.7860440826,94.7865211755072,3.04374365253442));
#27836=CARTESIAN_POINT('Ctrl Pts',(-185.51477702092,95.1132429797568,3.67482442913072));
#27837=CARTESIAN_POINT('Ctrl Pts',(-185.476427677548,95.5956987820616,4.26164147337986));
#27838=CARTESIAN_POINT('Ctrl Pts',(-185.635237128339,94.9678695342472,2.87648994589474));
#27839=CARTESIAN_POINT('Ctrl Pts',(-185.362056916117,95.2958407269429,3.47137285105012));
#27840=CARTESIAN_POINT('Ctrl Pts',(-185.304953205109,95.7685766079577,4.02746418701679));
#27841=CARTESIAN_POINT('Ctrl Pts',(-185.346408587176,95.3136337587549,2.51967239257564));
#27842=CARTESIAN_POINT('Ctrl Pts',(-185.069604964524,95.643921849378,3.03821885310616));
#27843=CARTESIAN_POINT('Ctrl Pts',(-184.97658882459,96.0979829082245,3.52787252597041));
#27844=CARTESIAN_POINT('Ctrl Pts',(-185.20795883318,95.4785673522034,2.32993303963118));
#27845=CARTESIAN_POINT('Ctrl Pts',(-184.929379865569,95.8100014195192,2.80832193017784));
#27846=CARTESIAN_POINT('Ctrl Pts',(-184.819211984195,96.2550053176917,3.26221242414813));
#27847=CARTESIAN_POINT('Ctrl Pts',(-184.949109662307,95.7857342654447,1.91734928765954));
#27848=CARTESIAN_POINT('Ctrl Pts',(-184.667275037263,96.1192146731736,2.30933190506252));
#27849=CARTESIAN_POINT('Ctrl Pts',(-184.525013064704,96.5472768103603,2.68454085282217));
#27850=CARTESIAN_POINT('Ctrl Pts',(-184.827448410629,95.9294455889528,1.69197258199757));
#27851=CARTESIAN_POINT('Ctrl Pts',(-184.544028383669,96.2639439959695,2.03717831284139));
#27852=CARTESIAN_POINT('Ctrl Pts',(-184.3867574195,96.6839296134637,2.36898381675622));
#27853=CARTESIAN_POINT('Ctrl Pts',(-184.673157550248,96.1111707509329,1.32666686830212));
#27854=CARTESIAN_POINT('Ctrl Pts',(-184.387725058793,96.4469529143824,1.59654749755515));
#27855=CARTESIAN_POINT('Ctrl Pts',(-184.21143808209,96.8566566608848,1.85750776184721));
#27856=CARTESIAN_POINT('Ctrl Pts',(-184.626384664622,96.1661612824647,1.20034830913053));
#27857=CARTESIAN_POINT('Ctrl Pts',(-184.340354066678,96.5023171881443,1.44433813660881));
#27858=CARTESIAN_POINT('Ctrl Pts',(-184.158293562368,96.9089107493774,1.68064518391667));
#27859=CARTESIAN_POINT('Ctrl Pts',(-184.544557060113,96.2622563647223,0.936341947650762));
#27860=CARTESIAN_POINT('Ctrl Pts',(-184.257494308414,96.5990477794699,1.12641432764746));
#27861=CARTESIAN_POINT('Ctrl Pts',(-184.065322417016,97.0002089202945,1.31100161190584));
#27862=CARTESIAN_POINT('Ctrl Pts',(-184.509590436998,96.3032573605489,0.798204058161918));
#27863=CARTESIAN_POINT('Ctrl Pts',(-184.222078190747,96.6403292797306,0.960133989517193));
#27864=CARTESIAN_POINT('Ctrl Pts',(-184.025595889726,97.0391546118712,1.11759042863826));
#27865=CARTESIAN_POINT('Ctrl Pts',(-184.456423260012,96.3655603217114,0.518880062316245));
#27866=CARTESIAN_POINT('Ctrl Pts',(-184.168239976604,96.7030436386975,0.624058853398732));
#27867=CARTESIAN_POINT('Ctrl Pts',(-183.96519246775,97.0983289670991,0.726500176433084));
#27868=CARTESIAN_POINT('Ctrl Pts',(-184.43780991789,96.3873480254583,0.376560788584548));
#27869=CARTESIAN_POINT('Ctrl Pts',(-184.149386424996,96.7249811721857,0.45285850256557));
#27870=CARTESIAN_POINT('Ctrl Pts',(-183.944046539593,97.1190192634854,0.527234512604526));
#27871=CARTESIAN_POINT('Ctrl Pts',(-184.418424799205,96.4100379276536,0.0859862665940266));
#27872=CARTESIAN_POINT('Ctrl Pts',(-184.129756564253,96.7478207757289,0.103410177548531));
#27873=CARTESIAN_POINT('Ctrl Pts',(-183.922023861298,97.1405661466642,0.120392057990099));
#27874=CARTESIAN_POINT('Ctrl Pts',(-184.417917263625,96.4106316699318,-0.0638962092285304));
#27875=CARTESIAN_POINT('Ctrl Pts',(-184.129242485696,96.7484185900842,-0.0768454065926074));
#27876=CARTESIAN_POINT('Ctrl Pts',(-183.921447280066,97.1411299348213,-0.0894630792312966));
#27877=CARTESIAN_POINT('Ctrl Pts',(-184.435598572149,96.3899366351428,-0.355921346913274));
#27878=CARTESIAN_POINT('Ctrl Pts',(-184.147147026983,96.7275870182977,-0.428034207439262));
#27879=CARTESIAN_POINT('Ctrl Pts',(-183.941534307246,97.1214775080755,-0.498336585883369));
#27880=CARTESIAN_POINT('Ctrl Pts',(-184.453495989889,96.3689882627064,-0.499360335068101));
#27881=CARTESIAN_POINT('Ctrl Pts',(-184.165275543997,96.7064944488072,-0.600578183941243));
#27882=CARTESIAN_POINT('Ctrl Pts',(-183.961866858988,97.1015844491156,-0.699169996799552));
#27883=CARTESIAN_POINT('Ctrl Pts',(-184.505728755164,96.3077846419852,-0.781557979895856));
#27884=CARTESIAN_POINT('Ctrl Pts',(-184.218167565914,96.6448867100655,-0.94010099938254));
#27885=CARTESIAN_POINT('Ctrl Pts',(-184.021208554627,97.0434548337247,-1.09428373408145));
#27886=CARTESIAN_POINT('Ctrl Pts',(-184.540234799446,96.2673269623919,-0.920237385586888));
#27887=CARTESIAN_POINT('Ctrl Pts',(-184.253117035716,96.6041524436365,-1.10702701224397));
#27888=CARTESIAN_POINT('Ctrl Pts',(-184.06041170346,97.0050256725195,-1.28845311054166));
#27889=CARTESIAN_POINT('Ctrl Pts',(-184.620686872807,96.1728572150355,-1.18387310682941));
#27890=CARTESIAN_POINT('Ctrl Pts',(-184.334583941818,96.5090579829018,-1.42449083732315));
#27891=CARTESIAN_POINT('Ctrl Pts',(-184.151819680695,96.9152730760786,-1.65757773666664));
#27892=CARTESIAN_POINT('Ctrl Pts',(-184.666866291424,96.1185715284399,-1.31029463806153));
#27893=CARTESIAN_POINT('Ctrl Pts',(-184.381354073376,96.454403175623,-1.5768166801151));
#27894=CARTESIAN_POINT('Ctrl Pts',(-184.204289665826,96.863689736492,-1.83458448860681));
#27895=CARTESIAN_POINT('Ctrl Pts',(-184.768797731556,95.9985328752646,-1.55440284628578));
#27896=CARTESIAN_POINT('Ctrl Pts',(-184.484570250941,96.3335691070844,-1.87111429108252));
#27897=CARTESIAN_POINT('Ctrl Pts',(-184.320112912034,96.7495971531963,-2.17636805559542));
#27898=CARTESIAN_POINT('Ctrl Pts',(-184.824880454895,95.932388707861,-1.67265647736271));
#27899=CARTESIAN_POINT('Ctrl Pts',(-184.541367291036,96.2669769912313,-2.0137851155555));
#27900=CARTESIAN_POINT('Ctrl Pts',(-184.383841997721,96.6867158385967,-2.34193868595053));
#27901=CARTESIAN_POINT('Ctrl Pts',(-185.002343333799,95.7226659996551,-2.01149464431596));
#27902=CARTESIAN_POINT('Ctrl Pts',(-184.721154715952,96.0557554309112,-2.42308663113885));
#27903=CARTESIAN_POINT('Ctrl Pts',(-184.585513418963,96.4872808224781,-2.81635673893943));
#27904=CARTESIAN_POINT('Ctrl Pts',(-185.132392337656,95.5684417093648,-2.21657750656061));
#27905=CARTESIAN_POINT('Ctrl Pts',(-184.852882048359,95.900452820441,-2.67111415072958));
#27906=CARTESIAN_POINT('Ctrl Pts',(-184.733319582232,96.3405488087457,-3.10349974620998));
#27907=CARTESIAN_POINT('Ctrl Pts',(-185.407131420796,95.2410911002814,-2.59999271242056));
#27908=CARTESIAN_POINT('Ctrl Pts',(-185.131072579201,95.5709154613594,-3.13562168059571));
#27909=CARTESIAN_POINT('Ctrl Pts',(-185.0456190211,96.028892389085,-3.64033156677099));
#27910=CARTESIAN_POINT('Ctrl Pts',(-185.55222076188,95.0674906005668,-2.77839835904419));
#27911=CARTESIAN_POINT('Ctrl Pts',(-185.278013603904,95.3961129331815,-3.35218099675058));
#27912=CARTESIAN_POINT('Ctrl Pts',(-185.210566100491,95.8635167264482,-3.89012301230439));
#27913=CARTESIAN_POINT('Ctrl Pts',(-185.851582277872,94.707494626045,-3.11437545164934));
#27914=CARTESIAN_POINT('Ctrl Pts',(-185.581125580994,95.0336977173119,-3.76083177968216));
#27915=CARTESIAN_POINT('Ctrl Pts',(-185.550953940504,95.5203349244564,-4.36053533295098));
#27916=CARTESIAN_POINT('Ctrl Pts',(-186.004341550726,94.5229247305643,-3.2702613765015));
#27917=CARTESIAN_POINT('Ctrl Pts',(-185.73581025216,94.8478641369735,-3.95083784102255));
#27918=CARTESIAN_POINT('Ctrl Pts',(-185.724674269717,95.344269925595,-4.57879624788273));
#27919=CARTESIAN_POINT('Ctrl Pts',(-186.468734209866,93.9589492331111,-3.71184473328433));
#27920=CARTESIAN_POINT('Ctrl Pts',(-186.206634192918,94.2793137095737,-4.49099146136749));
#27921=CARTESIAN_POINT('Ctrl Pts',(-186.252873560506,94.8059028848805,-5.19707165077033));
#27922=CARTESIAN_POINT('Ctrl Pts',(-186.786341213376,93.5694347474778,-3.97193417321456));
#27923=CARTESIAN_POINT('Ctrl Pts',(-186.528271047271,93.8870362158287,-4.81015854203247));
#27924=CARTESIAN_POINT('Ctrl Pts',(-186.614230377394,94.4335769026893,-5.56123140005082));
#27925=CARTESIAN_POINT('Ctrl Pts',(-187.429364224352,92.772219448936,-4.45009970653821));
#27926=CARTESIAN_POINT('Ctrl Pts',(-187.179275502702,93.0843625037761,-5.39983536323082));
#27927=CARTESIAN_POINT('Ctrl Pts',(-187.346070119741,93.6704353968611,-6.23072689748917));
#27928=CARTESIAN_POINT('Ctrl Pts',(-187.754922845355,92.3643571908662,-4.66770149404008));
#27929=CARTESIAN_POINT('Ctrl Pts',(-187.508904115674,92.6736124121426,-5.66953891705452));
#27930=CARTESIAN_POINT('Ctrl Pts',(-187.716714901687,93.2794672889775,-6.53539848906014));
#27931=CARTESIAN_POINT('Ctrl Pts',(-188.410112122538,91.5343223592301,-5.07270897607151));
#27932=CARTESIAN_POINT('Ctrl Pts',(-188.172164926541,91.8378317968073,-6.17425176407751));
#27933=CARTESIAN_POINT('Ctrl Pts',(-188.462886968343,92.4826689284514,-7.10246334796438));
#27934=CARTESIAN_POINT('Ctrl Pts',(-188.740497565809,91.1111729620599,-5.26033194798443));
#27935=CARTESIAN_POINT('Ctrl Pts',(-188.506622260807,91.4116871153395,-6.40936032306602));
#27936=CARTESIAN_POINT('Ctrl Pts',(-188.839274368838,92.0758984572259,-7.36516078216301));
#27937=CARTESIAN_POINT('Ctrl Pts',(-189.398843491069,90.2583421877452,-5.61022446203027));
#27938=CARTESIAN_POINT('Ctrl Pts',(-189.173011227327,90.5528941028731,-6.85041025678877));
#27939=CARTESIAN_POINT('Ctrl Pts',(-189.589532430357,91.2549207193099,-7.85505766520206));
#27940=CARTESIAN_POINT('Ctrl Pts',(-189.726873942438,89.8286042786326,-5.7725553986758));
#27941=CARTESIAN_POINT('Ctrl Pts',(-189.505024368188,90.1201178244939,-7.05626126941256));
#27942=CARTESIAN_POINT('Ctrl Pts',(-189.963481912788,90.8406631197547,-8.08234302955653));
#27943=CARTESIAN_POINT('Ctrl Pts',(-190.706530274547,88.5304660668642,-6.23019344512579));
#27944=CARTESIAN_POINT('Ctrl Pts',(-190.499557216329,88.8088485109363,-7.64207388345947));
#27945=CARTESIAN_POINT('Ctrl Pts',(-191.080632926279,89.5875778410458,-8.72309924440692));
#27946=CARTESIAN_POINT('Ctrl Pts',(-191.353674509396,87.6531907318376,-6.49656676606105));
#27947=CARTESIAN_POINT('Ctrl Pts',(-191.154383368923,87.9251930508971,-7.98648396265699));
#27948=CARTESIAN_POINT('Ctrl Pts',(-191.819082585706,88.7384854812239,-9.09605853590931));
#27949=CARTESIAN_POINT('Ctrl Pts',(-192.632970678399,85.8780091857335,-6.97723484386299));
#27950=CARTESIAN_POINT('Ctrl Pts',(-192.448889241933,86.1372754638322,-8.6170648745222));
#27951=CARTESIAN_POINT('Ctrl Pts',(-193.27977185066,87.0158621489936,-9.76906087244151));
#27952=CARTESIAN_POINT('Ctrl Pts',(-193.265161974548,84.9800606970277,-7.1911900404469));
#27953=CARTESIAN_POINT('Ctrl Pts',(-193.088386193258,85.2327644367758,-8.90204109889413));
#27954=CARTESIAN_POINT('Ctrl Pts',(-194.002055989696,86.1422915041419,-10.068628271248));
#27955=CARTESIAN_POINT('Ctrl Pts',(-195.136767560024,82.2575843111017,-7.77457663966346));
#27956=CARTESIAN_POINT('Ctrl Pts',(-194.993632951466,82.473345486734,-9.69714033640246));
#27957=CARTESIAN_POINT('Ctrl Pts',(-196.141646839768,83.4872301894655,-10.8854540504836));
#27958=CARTESIAN_POINT('Ctrl Pts',(-196.351118458959,80.4045345114431,-8.08647109199872));
#27959=CARTESIAN_POINT('Ctrl Pts',(-196.220621754019,80.6061801754008,-10.1354450942217));
#27960=CARTESIAN_POINT('Ctrl Pts',(-197.531576831738,81.6714982259837,-11.3221518808499));
#27961=CARTESIAN_POINT('Ctrl Pts',(-198.116766616771,77.5726081834688,-8.4814898062576));
#27962=CARTESIAN_POINT('Ctrl Pts',(-197.994458096547,77.7715661316189,-10.7114757703364));
#27963=CARTESIAN_POINT('Ctrl Pts',(-199.554667028181,78.8844065316243,-11.8752377009292));
#27964=CARTESIAN_POINT('Ctrl Pts',(-198.696041421195,76.6198655218917,-8.60067001276485));
#27965=CARTESIAN_POINT('Ctrl Pts',(-198.579787315131,76.8119296478313,-10.8906698919093));
#27966=CARTESIAN_POINT('Ctrl Pts',(-200.218774700134,77.9447528699897,-12.0421085545449));
#27967=CARTESIAN_POINT('Ctrl Pts',(-199.835393657519,74.6972603662356,-8.81827530517536));
#27968=CARTESIAN_POINT('Ctrl Pts',(-199.731156872596,74.8755477703346,-11.2265380697589));
#27969=CARTESIAN_POINT('Ctrl Pts',(-201.525656173084,76.0446910944109,-12.3467906967572));
#27970=CARTESIAN_POINT('Ctrl Pts',(-200.395927031185,73.7265427779827,-8.91674725157241));
#27971=CARTESIAN_POINT('Ctrl Pts',(-200.29727498786,73.8979510629713,-11.3829716214033));
#27972=CARTESIAN_POINT('Ctrl Pts',(-202.168953938337,75.0834314482927,-12.4846675143342));
#27973=CARTESIAN_POINT('Ctrl Pts',(-202.040776179842,70.8020841417172,-9.18473452855717));
#27974=CARTESIAN_POINT('Ctrl Pts',(-201.969429614348,70.9339332442469,-11.8248129171686));
#27975=CARTESIAN_POINT('Ctrl Pts',(-204.057598216847,72.1819343690171,-12.8598952638616));
#27976=CARTESIAN_POINT('Ctrl Pts',(-203.090555243157,68.8325136092258,-9.32755025230346));
#27977=CARTESIAN_POINT('Ctrl Pts',(-203.027559166486,68.9512781713152,-12.0764964747494));
#27978=CARTESIAN_POINT('Ctrl Pts',(-205.264224903837,70.2205205875485,-13.0598627591821));
#27979=CARTESIAN_POINT('Ctrl Pts',(-205.097425241471,64.8544500731044,-9.56200872917822));
#27980=CARTESIAN_POINT('Ctrl Pts',(-205.052948139998,64.9460837834979,-12.524607477045));
#27981=CARTESIAN_POINT('Ctrl Pts',(-207.572909482403,66.2457231416101,-13.3881499288596));
#27982=CARTESIAN_POINT('Ctrl Pts',(-206.054519269306,62.845953361298,-9.65350961790405));
#27983=CARTESIAN_POINT('Ctrl Pts',(-206.016439423784,62.9253694628212,-12.7190693605529));
#27984=CARTESIAN_POINT('Ctrl Pts',(-208.674970487123,64.2323356830512,-13.5162705613297));
#27985=CARTESIAN_POINT('Ctrl Pts',(-208.787453772969,56.7629489150811,-9.87162234708876));
#27986=CARTESIAN_POINT('Ctrl Pts',(-208.805906926216,56.7274477884812,-13.2469252044741));
#27987=CARTESIAN_POINT('Ctrl Pts',(-211.824237457266,58.1168549195064,-13.8216808903116));
#27988=CARTESIAN_POINT('Ctrl Pts',(-210.425226591334,52.631005892894,-9.94272536792823));
#27989=CARTESIAN_POINT('Ctrl Pts',(-210.440269997768,52.5822843956569,-13.5057475829278));
#27990=CARTESIAN_POINT('Ctrl Pts',(-213.714800431993,53.9395725306549,-13.9212498502496));
#27991=CARTESIAN_POINT('Ctrl Pts',(-212.604000467011,46.3190573027775,-9.9921716805904));
#27992=CARTESIAN_POINT('Ctrl Pts',(-212.606234394252,46.3108044017127,-13.8219499339134));
#27993=CARTESIAN_POINT('Ctrl Pts',(-216.232554404446,47.5307358639797,-13.9905049124008));
#27994=CARTESIAN_POINT('Ctrl Pts',(-213.283880548139,44.1960440918465,-9.99883242576813));
#27995=CARTESIAN_POINT('Ctrl Pts',(-213.287229079501,44.1810847215626,-13.9153550243481));
#27996=CARTESIAN_POINT('Ctrl Pts',(-217.018726572062,45.370602602594,-13.9998386774369));
#27997=CARTESIAN_POINT('Ctrl Pts',(-214.549838598837,39.9117037182066,-9.99904891274098));
#27998=CARTESIAN_POINT('Ctrl Pts',(-214.55760511708,39.8815809871525,-14.082597114446));
#27999=CARTESIAN_POINT('Ctrl Pts',(-218.483320257025,41.0034462363903,-14.0001571760684));
#28000=CARTESIAN_POINT('Ctrl Pts',(-215.136376568597,37.7485084112375,-9.99258580907847));
#28001=CARTESIAN_POINT('Ctrl Pts',(-215.143908548574,37.7144923110325,-14.1558384825482));
#28002=CARTESIAN_POINT('Ctrl Pts',(-219.162273921736,38.7945126487825,-13.991115461238));
#28003=CARTESIAN_POINT('Ctrl Pts',(-216.749953158185,31.2125703645965,-9.96182675340658));
#28004=CARTESIAN_POINT('Ctrl Pts',(-216.775802051944,31.100378487788,-14.3531964080252));
#28005=CARTESIAN_POINT('Ctrl Pts',(-221.030846972258,32.1103382810994,-13.9480701212897));
#28006=CARTESIAN_POINT('Ctrl Pts',(-217.620747415908,26.8377335828005,-9.92696743661106));
#28007=CARTESIAN_POINT('Ctrl Pts',(-217.634052712766,26.7487700574455,-14.4478056294438));
#28008=CARTESIAN_POINT('Ctrl Pts',(-222.040310058227,27.6230828990521,-13.899275220772));
#28009=CARTESIAN_POINT('Ctrl Pts',(-218.964732221164,18.0539614072054,-9.86263998637371));
#28010=CARTESIAN_POINT('Ctrl Pts',(-218.976069418789,17.9643982345151,-14.5927859676098));
#28011=CARTESIAN_POINT('Ctrl Pts',(-223.598907254315,18.5974327804109,-13.8092287551284));
#28012=CARTESIAN_POINT('Ctrl Pts',(-219.437897325133,13.6450084731965,-9.83311006111365));
#28013=CARTESIAN_POINT('Ctrl Pts',(-219.440263256372,13.5936991145387,-14.6404855064752));
#28014=CARTESIAN_POINT('Ctrl Pts',(-224.148014046288,14.0590074436304,-13.7678907295765));
#28015=CARTESIAN_POINT('Ctrl Pts',(-219.988849745161,4.79313733566884,-9.79797610395582));
#28016=CARTESIAN_POINT('Ctrl Pts',(-219.98909361829,4.7573196656202,-14.6968909906386));
#28017=CARTESIAN_POINT('Ctrl Pts',(-224.787432850351,4.94061146060701,-13.7187075789802));
#28018=CARTESIAN_POINT('Ctrl Pts',(-220.066648600991,0.350203291743644,
-9.79239486915522));
#28019=CARTESIAN_POINT('Ctrl Pts',(-220.065259345099,0.361024215332044,
-14.7045472577049));
#28020=CARTESIAN_POINT('Ctrl Pts',(-224.877757641866,0.360614518566908,
-13.7108944521662));
#28021=CARTESIAN_POINT('Ctrl Pts',(-219.881289785246,-6.34015037874837,
-9.80469728794968));
#28022=CARTESIAN_POINT('Ctrl Pts',(-219.880459455254,-6.32388335486397,
-14.6856874469098));
#28023=CARTESIAN_POINT('Ctrl Pts',(-224.662609304112,-6.53393892017589,
-13.7281163920661));
#28024=CARTESIAN_POINT('Ctrl Pts',(-219.7690846214,-8.5746040811491,-9.81212397201967));
#28025=CARTESIAN_POINT('Ctrl Pts',(-219.769195818231,-8.54934036973086,
-14.6743297915045));
#28026=CARTESIAN_POINT('Ctrl Pts',(-224.53237253079,-8.83622233241281,-13.7385128649179));
#28027=CARTESIAN_POINT('Ctrl Pts',(-219.441946243719,-13.0523359205035,
-9.83258686591823));
#28028=CARTESIAN_POINT('Ctrl Pts',(-219.443263597349,-13.0197708223219,
-14.6407181348838));
#28029=CARTESIAN_POINT('Ctrl Pts',(-224.152727496901,-13.4479084088541,
-13.767158287495));
#28030=CARTESIAN_POINT('Ctrl Pts',(-219.228078485099,-15.2805016753907,
-9.84554939701803));
#28031=CARTESIAN_POINT('Ctrl Pts',(-219.230954294149,-15.2408197429134,
-14.6187137573007));
#28032=CARTESIAN_POINT('Ctrl Pts',(-223.904556238525,-15.7417406054664,
-13.7853040799473));
#28033=CARTESIAN_POINT('Ctrl Pts',(-218.439133922489,-21.9259584225567,
-9.88922199339624));
#28034=CARTESIAN_POINT('Ctrl Pts',(-218.44812769664,-21.846612569119,-14.5362234536541));
#28035=CARTESIAN_POINT('Ctrl Pts',(-222.98929920683,-22.5783142290943,-13.8464389966528));
#28036=CARTESIAN_POINT('Ctrl Pts',(-217.716767444137,-26.3076453874502,
-9.92513263870734));
#28037=CARTESIAN_POINT('Ctrl Pts',(-217.737140154904,-26.2008567667317,
-14.460378345458));
#28038=CARTESIAN_POINT('Ctrl Pts',(-222.151504324182,-27.0796752766318,
-13.8967075271592));
#28039=CARTESIAN_POINT('Ctrl Pts',(-215.887601531786,-34.9758113643062,
-9.98260158823235));
#28040=CARTESIAN_POINT('Ctrl Pts',(-215.90681504924,-34.8830703988305,-14.2500621399759));
#28041=CARTESIAN_POINT('Ctrl Pts',(-220.03196646784,-35.9627273160852,-13.9771458586264));
#28042=CARTESIAN_POINT('Ctrl Pts',(-214.780781254865,-39.262299527481,-10.004263728387));
#28043=CARTESIAN_POINT('Ctrl Pts',(-214.811197566452,-39.1599104852413,
-14.1192077667389));
#28044=CARTESIAN_POINT('Ctrl Pts',(-218.750199620032,-40.344439125031,-14.007461154831));
#28045=CARTESIAN_POINT('Ctrl Pts',(-212.181660240525,-47.739771588893,-9.99138531231972));
#28046=CARTESIAN_POINT('Ctrl Pts',(-212.20113399609,-47.6723891640227,-13.7680488609868));
#28047=CARTESIAN_POINT('Ctrl Pts',(-215.743991965115,-48.9786473240517,
-13.9893987794769));
#28048=CARTESIAN_POINT('Ctrl Pts',(-210.689374656748,-51.9307717632098,
-9.95731215039984));
#28049=CARTESIAN_POINT('Ctrl Pts',(-210.715881161589,-51.8691066101861,
-13.5540230017111));
#28050=CARTESIAN_POINT('Ctrl Pts',(-214.019565211694,-53.2311754970819,
-13.9416762189794));
#28051=CARTESIAN_POINT('Ctrl Pts',(-208.153987483228,-58.143634952563,-9.81667719355973));
#28052=CARTESIAN_POINT('Ctrl Pts',(-208.131332303436,-58.1943415635481,
-13.1152950231644));
#28053=CARTESIAN_POINT('Ctrl Pts',(-211.0944995106,-59.5034442639553,-13.7447444436423));
#28054=CARTESIAN_POINT('Ctrl Pts',(-207.257503549638,-60.2058166920358,
-9.75447716181983));
#28055=CARTESIAN_POINT('Ctrl Pts',(-207.229900666133,-60.2678296059469,
-12.9529654277891));
#28056=CARTESIAN_POINT('Ctrl Pts',(-210.060944633878,-61.5799263735734,
-13.657648433114));
#28057=CARTESIAN_POINT('Ctrl Pts',(-205.378237956305,-64.273628314509,-9.58938880230249));
#28058=CARTESIAN_POINT('Ctrl Pts',(-205.334959986084,-64.3617609972516,
-12.5816370076419));
#28059=CARTESIAN_POINT('Ctrl Pts',(-207.896217583744,-65.663879283607,-13.4264876763358));
#28060=CARTESIAN_POINT('Ctrl Pts',(-204.394451399662,-66.2821759898736,
-9.48655954038466));
#28061=CARTESIAN_POINT('Ctrl Pts',(-204.344150257108,-66.3831240343329,
-12.3740275121672));
#28062=CARTESIAN_POINT('Ctrl Pts',(-206.763884251522,-67.6743142351468,
-13.2825059299792));
#28063=CARTESIAN_POINT('Ctrl Pts',(-202.339871295312,-70.2481208611195,
-9.22591917108276));
#28064=CARTESIAN_POINT('Ctrl Pts',(-202.270084276028,-70.3765254341986,
-11.8962907953015));
#28065=CARTESIAN_POINT('Ctrl Pts',(-204.401337671746,-71.6306725650387,
-12.9175609319477));
#28066=CARTESIAN_POINT('Ctrl Pts',(-201.269068012198,-72.2055260456701,
-9.06826451525565));
#28067=CARTESIAN_POINT('Ctrl Pts',(-201.190292857267,-72.347448988328,-11.6282123344199));
#28068=CARTESIAN_POINT('Ctrl Pts',(-203.171113874487,-73.5766035176501,
-12.6968171747456));
#28069=CARTESIAN_POINT('Ctrl Pts',(-199.041608375758,-76.068143900156,-8.67680213528545));
#28070=CARTESIAN_POINT('Ctrl Pts',(-198.939568678494,-76.2380118061437,
-11.0054857284394));
#28071=CARTESIAN_POINT('Ctrl Pts',(-200.614737956183,-77.4019017685666,
-12.1487056946224));
#28072=CARTESIAN_POINT('Ctrl Pts',(-197.884929568798,-77.9733779132744,
-8.44340949232921));
#28073=CARTESIAN_POINT('Ctrl Pts',(-197.771960106038,-78.1570310417782,
-10.6538744553092));
#28074=CARTESIAN_POINT('Ctrl Pts',(-199.288560854474,-79.2812891203015,
-11.8219197811625));
#28075=CARTESIAN_POINT('Ctrl Pts',(-196.086592698953,-80.7905481256368,
-8.00941122339776));
#28076=CARTESIAN_POINT('Ctrl Pts',(-195.942000534272,-81.0127720267323,
-10.0264388695469));
#28077=CARTESIAN_POINT('Ctrl Pts',(-197.229092539617,-82.0481576896257,
-11.2142562418261));
#28078=CARTESIAN_POINT('Ctrl Pts',(-195.476435527691,-81.7229977482265,
-7.85053630037284));
#28079=CARTESIAN_POINT('Ctrl Pts',(-195.325118084347,-81.9520318404096,
-9.80294658045898));
#28080=CARTESIAN_POINT('Ctrl Pts',(-196.530724565999,-82.9619066522144,
-10.9918079629887));
#28081=CARTESIAN_POINT('Ctrl Pts',(-194.240854639226,-83.5658540109184,
-7.49863854644174));
#28082=CARTESIAN_POINT('Ctrl Pts',(-194.075388956764,-83.8082449326526,
-9.31739070142719));
#28083=CARTESIAN_POINT('Ctrl Pts',(-195.117357931181,-84.7635976184135,
-10.499100026407));
#28084=CARTESIAN_POINT('Ctrl Pts',(-193.614824846021,-84.4772228383163,
-7.30555596453726));
#28085=CARTESIAN_POINT('Ctrl Pts',(-193.442219094693,-84.7263031125253,
-9.05574333461493));
#28086=CARTESIAN_POINT('Ctrl Pts',(-194.401665096834,-85.6524857281427,
-10.22875684803));
#28087=CARTESIAN_POINT('Ctrl Pts',(-192.347932759001,-86.2784285351058,
-6.87464479646914));
#28088=CARTESIAN_POINT('Ctrl Pts',(-192.160442100619,-86.5404947454048,
-8.48135963635239));
#28089=CARTESIAN_POINT('Ctrl Pts',(-192.954216968456,-87.4049400733434,
-9.62542037310025));
#28090=CARTESIAN_POINT('Ctrl Pts',(-191.707044521612,-87.1682928180243,
-6.63700210622506));
#28091=CARTESIAN_POINT('Ctrl Pts',(-191.512033111158,-87.4368721369655,
-8.16951011355977));
#28092=CARTESIAN_POINT('Ctrl Pts',(-192.222432355974,-88.2685319889458,
-9.29268753771301));
#28093=CARTESIAN_POINT('Ctrl Pts',(-190.378144990072,-88.9713989982768,
-6.08509931817266));
#28094=CARTESIAN_POINT('Ctrl Pts',(-190.167610974008,-89.2522458880518,
-7.45565276123948));
#28095=CARTESIAN_POINT('Ctrl Pts',(-190.706025517156,-90.0138628646082,
-8.51994753802441));
#28096=CARTESIAN_POINT('Ctrl Pts',(-189.689332036395,-89.8834557429178,
-5.76804029795621));
#28097=CARTESIAN_POINT('Ctrl Pts',(-189.470454598868,-90.1710185021602,
-7.05122460308101));
#28098=CARTESIAN_POINT('Ctrl Pts',(-189.920463440167,-90.8942884726876,
-8.07597136681174));
#28099=CARTESIAN_POINT('Ctrl Pts',(-188.996710505551,-90.7791921163431,
-5.39631620992176));
#28100=CARTESIAN_POINT('Ctrl Pts',(-188.764974135119,-91.0786621249365,
-6.58013865011089));
#28101=CARTESIAN_POINT('Ctrl Pts',(-189.131271676234,-91.7562941904943,
-7.55556514077405));
#28102=CARTESIAN_POINT('',(-189.102923332965,-90.6416650378459,-5.4533811546917));
#28103=CARTESIAN_POINT('',(-188.850942384682,90.9673968784445,5.31766757924549));
#28104=CARTESIAN_POINT('Ctrl Pts',(-189.102923332965,-90.641665037846,-5.4533811546917));
#28105=CARTESIAN_POINT('Ctrl Pts',(-189.582260717675,-90.020253446221,-5.70696955389192));
#28106=CARTESIAN_POINT('Ctrl Pts',(-190.058170492541,-89.3930857113232,
-5.93411277433641));
#28107=CARTESIAN_POINT('Ctrl Pts',(-190.53003087708,-88.7608183026999,-6.14212704225141));
#28108=CARTESIAN_POINT('Ctrl Pts',(-190.710986586798,-88.5183474333337,
-6.22189930268113));
#28109=CARTESIAN_POINT('Ctrl Pts',(-190.891347174418,-88.2751269204779,
-6.29885831045948));
#28110=CARTESIAN_POINT('Ctrl Pts',(-191.071079133441,-88.0311950960934,
-6.37341669810158));
#28111=CARTESIAN_POINT('Ctrl Pts',(-191.646252706304,-87.250570772353,-6.61201652442255));
#28112=CARTESIAN_POINT('Ctrl Pts',(-192.215025141179,-86.4626063253748,
-6.82549480142756));
#28113=CARTESIAN_POINT('Ctrl Pts',(-192.776838225234,-85.6678937138362,
-7.02043059393256));
#28114=CARTESIAN_POINT('Ctrl Pts',(-192.848364962895,-85.566715578091,-7.04524867255532));
#28115=CARTESIAN_POINT('Ctrl Pts',(-192.919778950195,-85.4654281068113,
-7.06976619818262));
#28116=CARTESIAN_POINT('Ctrl Pts',(-192.991079081859,-85.36403256041,-7.09399674750343));
#28117=CARTESIAN_POINT('Ctrl Pts',(-193.713446564455,-84.3367575205096,
-7.33948522706467));
#28118=CARTESIAN_POINT('Ctrl Pts',(-194.424096824214,-83.2984253835442,
-7.55590148935084));
#28119=CARTESIAN_POINT('Ctrl Pts',(-195.122436963889,-82.2496188764938,
-7.74993375843261));
#28120=CARTESIAN_POINT('Ctrl Pts',(-195.644764721679,-81.4651576661762,
-7.89506137503431));
#28121=CARTESIAN_POINT('Ctrl Pts',(-196.160206469516,-80.6748374593551,
-8.02766652837252));
#28122=CARTESIAN_POINT('Ctrl Pts',(-196.668528283489,-79.8789148564568,
-8.15054780740364));
#28123=CARTESIAN_POINT('Ctrl Pts',(-197.685784336456,-78.2861107248307,
-8.39645841256492));
#28124=CARTESIAN_POINT('Ctrl Pts',(-198.674593142452,-76.6707691018819,
-8.60245660480754));
#28125=CARTESIAN_POINT('Ctrl Pts',(-199.633903813475,-75.03378970395,-8.77941525971185));
#28126=CARTESIAN_POINT('Ctrl Pts',(-199.794861726751,-74.7591291628693,
-8.80910626252247));
#28127=CARTESIAN_POINT('Ctrl Pts',(-199.954989254821,-74.4838595913707,
-8.83797975018607));
#28128=CARTESIAN_POINT('Ctrl Pts',(-200.114281483532,-74.2079853746882,
-8.8660870801691));
#28129=CARTESIAN_POINT('Ctrl Pts',(-201.031953371716,-72.6186924419847,
-9.02801153050877));
#28130=CARTESIAN_POINT('Ctrl Pts',(-201.921922786274,-71.0093050648385,
-9.16424853724766));
#28131=CARTESIAN_POINT('Ctrl Pts',(-202.783481319878,-69.3802201617152,
-9.28065045514811));
#28132=CARTESIAN_POINT('Ctrl Pts',(-202.962805445657,-69.0411436919492,
-9.30487826016919));
#28133=CARTESIAN_POINT('Ctrl Pts',(-203.140898579713,-68.701213916756,-9.32824677071867));
#28134=CARTESIAN_POINT('Ctrl Pts',(-203.317754052504,-68.3604344681444,
-9.35080875744684));
#28135=CARTESIAN_POINT('Ctrl Pts',(-204.055553774916,-66.9387822081274,
-9.44493209602629));
#28136=CARTESIAN_POINT('Ctrl Pts',(-204.771821585756,-65.5023355039341,
-9.52494371021979));
#28137=CARTESIAN_POINT('Ctrl Pts',(-205.466126479309,-64.0511971714295,
-9.59344287612378));
#28138=CARTESIAN_POINT('Ctrl Pts',(-205.737857546834,-63.4832631529902,
-9.62025148952761));
#28139=CARTESIAN_POINT('Ctrl Pts',(-206.006223960639,-62.9130787823288,
-9.64529672325964));
#28140=CARTESIAN_POINT('Ctrl Pts',(-206.271197699333,-62.340650239919,-9.66873439603508));
#28141=CARTESIAN_POINT('Ctrl Pts',(-206.584024550177,-61.6648435764407,
-9.69640481123029));
#28142=CARTESIAN_POINT('Ctrl Pts',(-206.892247081492,-60.9856295693903,
-9.72182534319836));
#28143=CARTESIAN_POINT('Ctrl Pts',(-207.195451326658,-60.3038399562509,
-9.74517566651772));
#28144=CARTESIAN_POINT('Ctrl Pts',(-207.500367398821,-59.6182011032537,
-9.76865782082053));
#28145=CARTESIAN_POINT('Ctrl Pts',(-207.800208254404,-58.9299575759062,
-9.79004632456711));
#28146=CARTESIAN_POINT('Ctrl Pts',(-208.094601304795,-58.239977290383,-9.80952391276348));
#28147=CARTESIAN_POINT('Ctrl Pts',(-208.388994355186,-57.5499970048598,
-9.82900150095984));
#28148=CARTESIAN_POINT('Ctrl Pts',(-208.677939560999,-56.8582800885254,
-9.846568173606));
#28149=CARTESIAN_POINT('Ctrl Pts',(-208.961113653817,-56.1657146913821,
-9.86240666570794));
#28150=CARTESIAN_POINT('Ctrl Pts',(-209.495139736396,-54.8596348085616,
-9.89227581018714));
#28151=CARTESIAN_POINT('Ctrl Pts',(-210.009433697182,-53.5486516972336,
-9.9161782204413));
#28152=CARTESIAN_POINT('Ctrl Pts',(-210.504209260612,-52.2328373293754,
-9.93512269107262));
#28153=CARTESIAN_POINT('Ctrl Pts',(-211.00063112145,-50.9126447707905,-9.95413019681563));
#28154=CARTESIAN_POINT('Ctrl Pts',(-211.477404605655,-49.5875884934105,
-9.96814671432499));
#28155=CARTESIAN_POINT('Ctrl Pts',(-211.934701650502,-48.2577123828032,
-9.97819114162064));
#28156=CARTESIAN_POINT('Ctrl Pts',(-212.393661440177,-46.9230008055126,
-9.98827209073449));
#28157=CARTESIAN_POINT('Ctrl Pts',(-212.833003021567,-45.583434018586,-9.99435201185891));
#28158=CARTESIAN_POINT('Ctrl Pts',(-213.252854163575,-44.2390313383672,
-9.99746095769943));
#28159=CARTESIAN_POINT('Ctrl Pts',(-213.321782825185,-44.0183153079917,
-9.9979713659236));
#28160=CARTESIAN_POINT('Ctrl Pts',(-213.390186056062,-43.797468885728,-9.99840169710009));
#28161=CARTESIAN_POINT('Ctrl Pts',(-213.45806430009,-43.5764921004782,-9.99875650921472));
#28162=CARTESIAN_POINT('Ctrl Pts',(-213.878746211512,-42.2069673325635,
-10.0009554912408));
#28163=CARTESIAN_POINT('Ctrl Pts',(-214.279264487762,-40.8324457380546,
-10.0002042865536));
#28164=CARTESIAN_POINT('Ctrl Pts',(-214.659689264104,-39.4529486973177,
-9.9972139224554));
#28165=CARTESIAN_POINT('Ctrl Pts',(-215.059027314902,-38.0048683051126,
-9.99407488881614));
#28166=CARTESIAN_POINT('Ctrl Pts',(-215.436224812888,-36.5513052574736,
-9.98846851623776));
#28167=CARTESIAN_POINT('Ctrl Pts',(-215.791304305115,-35.0922648472616,
-9.98121724046361));
#28168=CARTESIAN_POINT('Ctrl Pts',(-216.146383797341,-33.6332244370496,
-9.97396596468947));
#28169=CARTESIAN_POINT('Ctrl Pts',(-216.479345374389,-32.1687062920674,
-9.96506978571955));
#28170=CARTESIAN_POINT('Ctrl Pts',(-216.79015016326,-30.6987012818522,-9.95535113929721));
#28171=CARTESIAN_POINT('Ctrl Pts',(-217.083045980536,-29.3133998505938,
-9.94619249377886));
#28172=CARTESIAN_POINT('Ctrl Pts',(-217.356262700494,-27.9232340571749,
-9.93629265774494));
#28173=CARTESIAN_POINT('Ctrl Pts',(-217.609720097247,-26.5281727798487,
-9.92610877818971));
#28174=CARTESIAN_POINT('Ctrl Pts',(-217.862641171742,-25.1360634874478,
-9.91594644798103));
#28175=CARTESIAN_POINT('Ctrl Pts',(-218.095886491803,-23.7390791164929,
-9.90550127506577));
#28176=CARTESIAN_POINT('Ctrl Pts',(-218.309324573698,-22.3371857234748,
-9.8952275105708));
#28177=CARTESIAN_POINT('Ctrl Pts',(-218.521921535319,-20.9408169348002,
-9.88499423309448));
#28178=CARTESIAN_POINT('Ctrl Pts',(-218.714867074954,-19.5395774505493,
-9.87493101572222));
#28179=CARTESIAN_POINT('Ctrl Pts',(-218.887979530425,-18.1334350540361,
-9.86548676035596));
#28180=CARTESIAN_POINT('Ctrl Pts',(-218.912596242757,-17.9334806210731,
-9.86414378063271));
#28181=CARTESIAN_POINT('Ctrl Pts',(-218.936811823662,-17.7334270525466,
-9.86281331696435));
#28182=CARTESIAN_POINT('Ctrl Pts',(-218.960625665239,-17.5332742632934,
-9.86149666014403));
#28183=CARTESIAN_POINT('Ctrl Pts',(-219.184812192997,-15.6490104959437,
-9.84910148568848));
#28184=CARTESIAN_POINT('Ctrl Pts',(-219.373454863963,-13.7554245499718,
-9.83785494815097));
#28185=CARTESIAN_POINT('Ctrl Pts',(-219.525841126991,-11.8536894372336,
-9.82845661547209));
#28186=CARTESIAN_POINT('Ctrl Pts',(-219.552867756293,-11.5164051643565,
-9.82678976408852));
#28187=CARTESIAN_POINT('Ctrl Pts',(-219.578753985703,-11.1788646797448,
-9.8251810483157));
#28188=CARTESIAN_POINT('Ctrl Pts',(-219.603495908495,-10.8410746855513,
-9.82363437087996));
#28189=CARTESIAN_POINT('Ctrl Pts',(-219.705373439927,-9.45018800954576,
-9.81726575998433));
#28190=CARTESIAN_POINT('Ctrl Pts',(-219.787419394757,-8.06100294968608,
-9.81197810113728));
#28191=CARTESIAN_POINT('Ctrl Pts',(-219.849875987437,-6.6735051628098,-9.80789674793111));
#28192=CARTESIAN_POINT('Ctrl Pts',(-219.888111421962,-5.82408993686036,
-9.80539817561728));
#28193=CARTESIAN_POINT('Ctrl Pts',(-219.919004199351,-4.97530671931527,
-9.80335170157182));
#28194=CARTESIAN_POINT('Ctrl Pts',(-219.942600668612,-4.12714946555835,
-9.80178608653178));
#28195=CARTESIAN_POINT('Ctrl Pts',(-219.982142675654,-2.70584190766221,
-9.79916249228756));
#28196=CARTESIAN_POINT('Ctrl Pts',(-220.001198185544,-1.28628743268108,
-9.79793805992874));
#28197=CARTESIAN_POINT('Ctrl Pts',(-219.999941724939,0.131516457556867,
-9.79805476787017));
#28198=CARTESIAN_POINT('Ctrl Pts',(-219.998682147343,1.55283759632288,-9.79817176533743));
#28199=CARTESIAN_POINT('Ctrl Pts',(-219.977009716239,2.97239974751487,-9.79963656548587));
#28200=CARTESIAN_POINT('Ctrl Pts',(-219.935048547014,4.3902139918877,-9.80239071384323));
#28201=CARTESIAN_POINT('Ctrl Pts',(-219.892987902636,5.81138937446998,-9.80515139131631));
#28202=CARTESIAN_POINT('Ctrl Pts',(-219.830542222622,7.23080884893533,-9.80920753742537));
#28203=CARTESIAN_POINT('Ctrl Pts',(-219.74778437218,8.64848773576876,-9.81450028098692));
#28204=CARTESIAN_POINT('Ctrl Pts',(-219.736609773761,8.83991359037877,-9.81521494773474));
#28205=CARTESIAN_POINT('Ctrl Pts',(-219.725064756642,9.03130771205525,-9.81595216070532));
#28206=CARTESIAN_POINT('Ctrl Pts',(-219.713149427464,9.22267013971849,-9.81671177496444));
#28207=CARTESIAN_POINT('Ctrl Pts',(-219.624287664256,10.6498067701466,-9.82237680204124));
#28208=CARTESIAN_POINT('Ctrl Pts',(-219.514834598448,12.0751717546752,-9.82928536128041));
#28209=CARTESIAN_POINT('Ctrl Pts',(-219.38480626819,13.4987695466866,-9.83712441968859));
#28210=CARTESIAN_POINT('Ctrl Pts',(-219.254821792827,14.9218871992416,-9.84496083420306));
#28211=CARTESIAN_POINT('Ctrl Pts',(-219.104275899337,16.3432391502397,-9.85372712033006));
#28212=CARTESIAN_POINT('Ctrl Pts',(-218.933132808931,17.7628245558423,-9.86311056170108));
#28213=CARTESIAN_POINT('Ctrl Pts',(-218.762257656336,19.1801874901504,-9.87247931256528));
#28214=CARTESIAN_POINT('Ctrl Pts',(-218.570849700195,20.5957897010906,-9.88246328777715));
#28215=CARTESIAN_POINT('Ctrl Pts',(-218.358822292918,22.0096206245496,-9.89275123741531));
#28216=CARTESIAN_POINT('Ctrl Pts',(-218.335813724675,22.1630452487734,-9.89386765436523));
#28217=CARTESIAN_POINT('Ctrl Pts',(-218.312562294107,22.3164490024472,-9.89498765089645));
#28218=CARTESIAN_POINT('Ctrl Pts',(-218.289067854669,22.4698318628755,-9.89611082926645));
#28219=CARTESIAN_POINT('Ctrl Pts',(-218.077188114775,23.8530834470226,-9.90623998095426));
#28220=CARTESIAN_POINT('Ctrl Pts',(-217.845550020112,25.2346280157213,-9.91663409193066));
#28221=CARTESIAN_POINT('Ctrl Pts',(-217.594014743781,26.6144719940167,-9.92675978258888));
#28222=CARTESIAN_POINT('Ctrl Pts',(-217.343223872589,27.9902323981778,-9.93685550680951));
#28223=CARTESIAN_POINT('Ctrl Pts',(-217.072653340494,29.3643025370337,-9.94668439711208));
#28224=CARTESIAN_POINT('Ctrl Pts',(-216.782117050876,30.736670744236,-9.955717795414));
#28225=CARTESIAN_POINT('Ctrl Pts',(-216.493058233207,32.1020600107562,-9.96470525593437));
#28226=CARTESIAN_POINT('Ctrl Pts',(-216.184236108853,33.4657648725542,-9.97290529455565));
#28227=CARTESIAN_POINT('Ctrl Pts',(-215.855420636239,34.8277519779683,-9.97979727744779));
#28228=CARTESIAN_POINT('Ctrl Pts',(-215.792138141171,35.0898745040037,-9.98112368058178));
#28229=CARTESIAN_POINT('Ctrl Pts',(-215.728114969485,35.3519333335032,-9.98240163425538));
#28230=CARTESIAN_POINT('Ctrl Pts',(-215.663349285992,35.6139281225462,-9.98362742716542));
#28231=CARTESIAN_POINT('Ctrl Pts',(-215.378618518289,36.7657414501431,-9.98901640690739));
#28232=CARTESIAN_POINT('Ctrl Pts',(-215.080318928169,37.9131343588526,-9.9933404843776));
#28233=CARTESIAN_POINT('Ctrl Pts',(-214.768739822526,39.0553552393069,-9.99618853751749));
#28234=CARTESIAN_POINT('Ctrl Pts',(-214.490069922121,40.0769339434976,-9.99873577727286));
#28235=CARTESIAN_POINT('Ctrl Pts',(-214.200778251147,41.094375598618,-10.0001023240286));
#28236=CARTESIAN_POINT('Ctrl Pts',(-213.901104808522,42.1071550347656,-9.99999405004369));
#28237=CARTESIAN_POINT('Ctrl Pts',(-213.492922283981,43.4866528755784,-9.99984657101419));
#28238=CARTESIAN_POINT('Ctrl Pts',(-213.065281545394,44.8581999124421,-9.99697039599626));
#28239=CARTESIAN_POINT('Ctrl Pts',(-212.618337105391,46.2218293651797,-9.99049076100407));
#28240=CARTESIAN_POINT('Ctrl Pts',(-212.370269085231,46.9786859860388,-9.98689436270485));
#28241=CARTESIAN_POINT('Ctrl Pts',(-212.116253451429,47.733103416628,-9.98218788464245));
#28242=CARTESIAN_POINT('Ctrl Pts',(-211.856309787049,48.4850862480963,-9.97622175746237));
#28243=CARTESIAN_POINT('Ctrl Pts',(-211.379488601213,49.8644672239142,-9.96527794067941));
#28244=CARTESIAN_POINT('Ctrl Pts',(-210.882722773809,51.2356606005683,-9.95022000519016));
#28245=CARTESIAN_POINT('Ctrl Pts',(-210.36610102331,52.5986610272489,-9.92976988604603));
#28246=CARTESIAN_POINT('Ctrl Pts',(-209.835337069147,53.9989727549137,-9.9087599574289));
#28247=CARTESIAN_POINT('Ctrl Pts',(-209.283615347521,55.3906372337196,-9.88205858904313));
#28248=CARTESIAN_POINT('Ctrl Pts',(-208.710977413956,56.7736317201052,-9.84827985780893));
#28249=CARTESIAN_POINT('Ctrl Pts',(-208.138339480391,58.1566262064908,-9.81450112657472));
#28250=CARTESIAN_POINT('Ctrl Pts',(-207.54478519928,59.5309510279822,-9.77364503249207));
#28251=CARTESIAN_POINT('Ctrl Pts',(-206.930302679868,60.8965613623573,-9.72432565248121));
#28252=CARTESIAN_POINT('Ctrl Pts',(-206.32754650778,62.2361113604596,-9.67594744843798));
#28253=CARTESIAN_POINT('Ctrl Pts',(-205.704653571512,63.5672747476244,-9.61968076721895));
#28254=CARTESIAN_POINT('Ctrl Pts',(-205.061572025718,64.8899703091143,-9.55306338132051));
#28255=CARTESIAN_POINT('Ctrl Pts',(-204.408458319862,66.2333001022554,-9.48540675509146));
#28256=CARTESIAN_POINT('Ctrl Pts',(-203.734521172266,67.5678961860887,-9.40707396037423));
#28257=CARTESIAN_POINT('Ctrl Pts',(-203.039660016423,68.8936434234688,-9.31548572940536));
#28258=CARTESIAN_POINT('Ctrl Pts',(-202.34479886058,70.2193906608489,-9.22389749843649));
#28259=CARTESIAN_POINT('Ctrl Pts',(-201.629013533948,71.5362893553416,-9.11905383121599));
#28260=CARTESIAN_POINT('Ctrl Pts',(-200.892159193484,72.8441895279559,-8.99837545998041));
#28261=CARTESIAN_POINT('Ctrl Pts',(-200.586970936635,73.3858919403522,-8.94839323183244));
#28262=CARTESIAN_POINT('Ctrl Pts',(-200.278025369755,73.9262941980819,-8.89557299390327));
#28263=CARTESIAN_POINT('Ctrl Pts',(-199.965848931004,74.4644603316202,-8.83971192769632));
#28264=CARTESIAN_POINT('Ctrl Pts',(-199.715624687529,74.8958260495664,-8.79493662983211));
#28265=CARTESIAN_POINT('Ctrl Pts',(-199.463325568433,75.3257555676997,-8.7482076655061));
#28266=CARTESIAN_POINT('Ctrl Pts',(-199.209243550892,75.7537790987561,-8.69942058786797));
#28267=CARTESIAN_POINT('Ctrl Pts',(-198.638172186973,76.7157990954304,-8.5897674009244));
#28268=CARTESIAN_POINT('Ctrl Pts',(-198.057534390405,77.6691493924228,-8.46965732294354));
#28269=CARTESIAN_POINT('Ctrl Pts',(-197.467674066489,78.6136055049731,-8.33695469259649));
#28270=CARTESIAN_POINT('Ctrl Pts',(-196.830489808791,79.6338344347796,-8.19360545620275));
#28271=CARTESIAN_POINT('Ctrl Pts',(-196.182500603122,80.6437484421905,-8.03598349849812));
#28272=CARTESIAN_POINT('Ctrl Pts',(-195.524339684909,81.6427983389507,-7.85954724113827));
#28273=CARTESIAN_POINT('Ctrl Pts',(-194.963942524463,82.4934485519824,-7.70931896886041));
#28274=CARTESIAN_POINT('Ctrl Pts',(-194.39617173317,83.3362230411495,-7.54545065392799));
#28275=CARTESIAN_POINT('Ctrl Pts',(-193.821438603718,84.1708044967981,-7.36513881081726));
#28276=CARTESIAN_POINT('Ctrl Pts',(-193.278404315604,84.9593554318606,-7.19477189033818));
#28277=CARTESIAN_POINT('Ctrl Pts',(-192.729171431316,85.7405634546523,-7.00954588434748));
#28278=CARTESIAN_POINT('Ctrl Pts',(-192.174344836506,86.5138551176446,-6.8048710633828));
#28279=CARTESIAN_POINT('Ctrl Pts',(-192.090736617309,86.6303843890734,-6.7740280982918));
#28280=CARTESIAN_POINT('Ctrl Pts',(-192.007001446041,86.7467339588819,-6.74274348491311));
#28281=CARTESIAN_POINT('Ctrl Pts',(-191.923141467766,86.862901934308,-6.71100151736954));
#28282=CARTESIAN_POINT('Ctrl Pts',(-191.455364919845,87.5108946436029,-6.53394270687155));
#28283=CARTESIAN_POINT('Ctrl Pts',(-190.983682123568,88.1532614843595,-6.34284056508145));
#28284=CARTESIAN_POINT('Ctrl Pts',(-190.508729882859,88.7893533408363,-6.13265396746052));
#28285=CARTESIAN_POINT('Ctrl Pts',(-190.333501788842,89.0240320181371,-6.05510807182643));
#28286=CARTESIAN_POINT('Ctrl Pts',(-190.157829060128,89.2578569081404,-5.97496448588751));
#28287=CARTESIAN_POINT('Ctrl Pts',(-189.981745013892,89.4907965997159,-5.89197005329973));
#28288=CARTESIAN_POINT('Ctrl Pts',(-189.655066849744,89.9229556307455,-5.73799546302966));
#28289=CARTESIAN_POINT('Ctrl Pts',(-189.326983490681,90.3520514824435,-5.57410111969077));
#28290=CARTESIAN_POINT('Ctrl Pts',(-188.997857715772,90.7777088121816,-5.3973851824285));
#28291=CARTESIAN_POINT('Ctrl Pts',(-188.775987395932,91.0646529991488,-5.27825740663509));
#28292=CARTESIAN_POINT('Ctrl Pts',(-188.553790413721,91.3498385361321,-5.1533706364117));
#28293=CARTESIAN_POINT('Ctrl Pts',(-188.332426130858,91.6318520768341,-5.02200062463247));
#28294=CARTESIAN_POINT('Ctrl Pts',(-188.225415301687,91.7681816709206,-4.95849438185974));
#28295=CARTESIAN_POINT('Ctrl Pts',(-188.118599682122,91.9037704920273,-4.89347306955748));
#28296=CARTESIAN_POINT('Ctrl Pts',(-188.012113626743,92.0384616157055,-4.82685487001534));
#28297=CARTESIAN_POINT('Ctrl Pts',(-187.746746782362,92.3741164423341,-4.66084006809688));
#28298=CARTESIAN_POINT('Ctrl Pts',(-187.482921186823,92.7048308672381,-4.48476227846315));
#28299=CARTESIAN_POINT('Ctrl Pts',(-187.221786938517,93.029395239841,-4.29514604930913));
#28300=CARTESIAN_POINT('Ctrl Pts',(-187.16136829591,93.1044897131185,-4.25127453396387));
#28301=CARTESIAN_POINT('Ctrl Pts',(-187.101093892561,93.1792551071998,-4.20667827755538));
#28302=CARTESIAN_POINT('Ctrl Pts',(-187.040978266996,93.2536767007252,-4.16131423409769));
#28303=CARTESIAN_POINT('Ctrl Pts',(-186.822264168965,93.5244391114808,-3.99626969277047));
#28304=CARTESIAN_POINT('Ctrl Pts',(-186.60557949658,93.790733324454,-3.82129133643407));
#28305=CARTESIAN_POINT('Ctrl Pts',(-186.392328671109,94.0510234661448,-3.63203987613659));
#28306=CARTESIAN_POINT('Ctrl Pts',(-186.293631092486,94.1714919645312,-3.54444977729014));
#28307=CARTESIAN_POINT('Ctrl Pts',(-186.195669634349,94.2906748481443,-3.45380229447933));
#28308=CARTESIAN_POINT('Ctrl Pts',(-186.098586341438,94.4084223188913,-3.35966723216558));
#28309=CARTESIAN_POINT('Ctrl Pts',(-185.966190956342,94.5689980602577,-3.23129243715974));
#28310=CARTESIAN_POINT('Ctrl Pts',(-185.834880990427,94.7275622180069,-3.09597884224675));
#28311=CARTESIAN_POINT('Ctrl Pts',(-185.706791881215,94.8816114060829,-2.95260056874952));
#28312=CARTESIAN_POINT('Ctrl Pts',(-185.572843211037,95.042707724199,-2.8026633165852));
#28313=CARTESIAN_POINT('Ctrl Pts',(-185.442416968954,95.1988666121742,-2.64390665578969));
#28314=CARTESIAN_POINT('Ctrl Pts',(-185.317999081605,95.3472624190148,-2.4750430182964));
#28315=CARTESIAN_POINT('Ctrl Pts',(-185.285649188078,95.3858468111261,-2.43113678576129));
#28316=CARTESIAN_POINT('Ctrl Pts',(-185.25370570196,95.4239065608026,-2.38654726910167));
#28317=CARTESIAN_POINT('Ctrl Pts',(-185.22221274141,95.4613923628908,-2.3412518354128));
#28318=CARTESIAN_POINT('Ctrl Pts',(-185.100635614399,95.6061045792706,-2.16639089511405));
#28319=CARTESIAN_POINT('Ctrl Pts',(-184.98542456809,95.7426706963575,-1.98055943370035));
#28320=CARTESIAN_POINT('Ctrl Pts',(-184.880016161317,95.867230027294,-1.7782718643602));
#28321=CARTESIAN_POINT('Ctrl Pts',(-184.869055232791,95.8801823710909,-1.75723692362779));
#28322=CARTESIAN_POINT('Ctrl Pts',(-184.858200333914,95.8930049161292,-1.73602404382374));
#28323=CARTESIAN_POINT('Ctrl Pts',(-184.847455350633,95.905693340827,-1.71462705701883));
#28324=CARTESIAN_POINT('Ctrl Pts',(-184.733378649987,96.0404030549373,-1.48746079769588));
#28325=CARTESIAN_POINT('Ctrl Pts',(-184.634606015397,96.15654553355,-1.24506065412383));
#28326=CARTESIAN_POINT('Ctrl Pts',(-184.559925794379,96.2441998630232,-0.982882582956073));
#28327=CARTESIAN_POINT('Ctrl Pts',(-184.522585683869,96.2880270277597,-0.851793547372224));
#28328=CARTESIAN_POINT('Ctrl Pts',(-184.491200496658,96.3248129826987,-0.71446995864745));
#28329=CARTESIAN_POINT('Ctrl Pts',(-184.468141456029,96.3518258459007,-0.575828787863998));
#28330=CARTESIAN_POINT('Ctrl Pts',(-184.445082415399,96.3788387091026,-0.437187617080504));
#28331=CARTESIAN_POINT('Ctrl Pts',(-184.430008139983,96.3964802963479,-0.29639152936448));
#28332=CARTESIAN_POINT('Ctrl Pts',(-184.423682240228,96.4038839485828,-0.153238376079624));
#28333=CARTESIAN_POINT('Ctrl Pts',(-184.417356340473,96.4112876008179,-0.0100852227948052));
#28334=CARTESIAN_POINT('Ctrl Pts',(-184.42006841148,96.408114875489,0.135625753676425));
#28335=CARTESIAN_POINT('Ctrl Pts',(-184.43135369862,96.3949047695855,0.276911155354654));
#28336=CARTESIAN_POINT('Ctrl Pts',(-184.442638985761,96.3816946636821,0.418196557032899));
#28337=CARTESIAN_POINT('Ctrl Pts',(-184.462339979552,96.3586308331086,0.556826534586012));
#28338=CARTESIAN_POINT('Ctrl Pts',(-184.489631932353,96.3266448140663,0.69305600086679));
#28339=CARTESIAN_POINT('Ctrl Pts',(-184.516923885154,96.294658795024,0.829285467147568));
#28340=CARTESIAN_POINT('Ctrl Pts',(-184.552177704994,96.2533138975323,0.964043576315172));
#28341=CARTESIAN_POINT('Ctrl Pts',(-184.5930207893,96.2053417784222,1.09284689451645));
#28342=CARTESIAN_POINT('Ctrl Pts',(-184.633863873607,96.1573696593121,1.22165021271772));
#28343=CARTESIAN_POINT('Ctrl Pts',(-184.680332525911,96.1027279897818,1.3452763845494));
#28344=CARTESIAN_POINT('Ctrl Pts',(-184.731342004596,96.0426400031113,1.46469528137978));
#28345=CARTESIAN_POINT('Ctrl Pts',(-184.806244825786,95.9544062113289,1.64005116633558));
#28346=CARTESIAN_POINT('Ctrl Pts',(-184.890988249303,95.8543655363102,1.80625356976928));
#28347=CARTESIAN_POINT('Ctrl Pts',(-184.981448115991,95.7472408523625,1.96283299189215));
#28348=CARTESIAN_POINT('Ctrl Pts',(-185.014196175743,95.7084598362128,2.0195174914331));
#28349=CARTESIAN_POINT('Ctrl Pts',(-185.047693759096,95.6687507118301,2.07494083470269));
#28350=CARTESIAN_POINT('Ctrl Pts',(-185.081746563357,95.6283387304002,2.12908074636339));
#28351=CARTESIAN_POINT('Ctrl Pts',(-185.209863326123,95.476296854548,2.33277117271976));
#28352=CARTESIAN_POINT('Ctrl Pts',(-185.347035066172,95.3128818079577,2.52072565082259));
#28353=CARTESIAN_POINT('Ctrl Pts',(-185.490287760292,95.1413922088622,2.69775019367684));
#28354=CARTESIAN_POINT('Ctrl Pts',(-185.6117572313,94.9959795797082,2.84785611460146));
#28355=CARTESIAN_POINT('Ctrl Pts',(-185.738091612429,94.844170547157,2.99046782053365));
#28356=CARTESIAN_POINT('Ctrl Pts',(-185.866969235358,94.6886391437972,3.12595992617305));
#28357=CARTESIAN_POINT('Ctrl Pts',(-185.890080968629,94.6607475655074,3.15025784023058));
#28358=CARTESIAN_POINT('Ctrl Pts',(-185.913274594529,94.6327363650839,3.17432679112757));
#28359=CARTESIAN_POINT('Ctrl Pts',(-185.936536862367,94.6046210817755,3.19816893934182));
#28360=CARTESIAN_POINT('Ctrl Pts',(-186.132399677713,94.3678970193877,3.39891421085154));
#28361=CARTESIAN_POINT('Ctrl Pts',(-186.33318700497,94.1237178420589,3.58426602215573));
#28362=CARTESIAN_POINT('Ctrl Pts',(-186.537347521913,93.8737371558285,3.7581436355622));
#28363=CARTESIAN_POINT('Ctrl Pts',(-186.652107529757,93.7332213208283,3.85588141844489));
#28364=CARTESIAN_POINT('Ctrl Pts',(-186.767934004726,93.5908730084738,3.94999376768016));
#28365=CARTESIAN_POINT('Ctrl Pts',(-186.884556928866,93.4469907241288,4.04117676585312));
#28366=CARTESIAN_POINT('Ctrl Pts',(-187.102775149859,93.1777663297489,4.21179323592527));
#28367=CARTESIAN_POINT('Ctrl Pts',(-187.322831812982,92.9043391410468,4.37109190838243));
#28368=CARTESIAN_POINT('Ctrl Pts',(-187.543491073221,92.6281267656026,4.52125345487312));
#28369=CARTESIAN_POINT('Ctrl Pts',(-187.650554852589,92.4941086383265,4.5941117734665));
#28370=CARTESIAN_POINT('Ctrl Pts',(-187.757761085074,92.3594353231351,4.6648190424016));
#28371=CARTESIAN_POINT('Ctrl Pts',(-187.864972028382,92.2242715800883,4.73362434893738));
#28372=CARTESIAN_POINT('Ctrl Pts',(-188.193145537924,91.8105343388161,4.94423791341334));
#28373=CARTESIAN_POINT('Ctrl Pts',(-188.522111622863,91.3912547978073,5.13734380348656));
#28374=CARTESIAN_POINT('Ctrl Pts',(-188.850942384682,90.9673968784446,5.31766757924549));
#28375=CARTESIAN_POINT('Origin',(-192.01137155147,93.4192711577907,5.31766757925036));
#28376=CARTESIAN_POINT('Origin',(-192.27014422543,-93.0847597593693,-5.4533811546917));
#28377=CARTESIAN_POINT('Origin',(0.,-222.,0.));
#28378=CARTESIAN_POINT('',(199.738310248729,-222.,14.));
#28379=CARTESIAN_POINT('',(0.,-222.,14.));
#28380=CARTESIAN_POINT('Origin',(199.738310248729,-222.,0.));
#28381=CARTESIAN_POINT('Origin',(199.738310248729,222.,0.));
#28382=CARTESIAN_POINT('',(199.738310248729,222.,-14.));
#28383=CARTESIAN_POINT('Origin',(199.738310248729,222.,0.));
#28384=CARTESIAN_POINT('',(199.738310248729,222.,-14.));
#28385=CARTESIAN_POINT('Ctrl Pts',(-188.311118109849,-90.0308913574651,
-5.4533811546917));
#28386=CARTESIAN_POINT('Ctrl Pts',(-188.023256533701,-90.4040742676823,
-6.95129107926417));
#28387=CARTESIAN_POINT('Ctrl Pts',(-188.497959509479,-91.2585968975267,
-8.18023862635663));
#28388=CARTESIAN_POINT('Ctrl Pts',(-187.982864381004,-90.4564385369785,
-5.27854386264169));
#28389=CARTESIAN_POINT('Ctrl Pts',(-187.690945735358,-90.8320759397691,
-6.72011486605825));
#28390=CARTESIAN_POINT('Ctrl Pts',(-188.112012071841,-91.6642006348184,
-7.91797096057072));
#28391=CARTESIAN_POINT('Ctrl Pts',(-187.655409171816,-90.876129304024,-5.09218567437125));
#28392=CARTESIAN_POINT('Ctrl Pts',(-187.3584086985,-91.2554874222619,-6.4746919750007));
#28393=CARTESIAN_POINT('Ctrl Pts',(-187.72718172021,-92.0634779561488,-7.6384374977848));
#28394=CARTESIAN_POINT('Ctrl Pts',(-187.004381777406,-91.7014919148641,
-4.68919575393491));
#28395=CARTESIAN_POINT('Ctrl Pts',(-186.697275840756,-92.0880272032448,
-5.94749868714714));
#28396=CARTESIAN_POINT('Ctrl Pts',(-186.962365167593,-92.8473379257022,
-7.03394292888026));
#28397=CARTESIAN_POINT('Ctrl Pts',(-186.680764536156,-92.1072147831329,
-4.47270326949046));
#28398=CARTESIAN_POINT('Ctrl Pts',(-186.368574011069,-92.4973363451042,
-5.66609145238058));
#28399=CARTESIAN_POINT('Ctrl Pts',(-186.582338053018,-93.2319556715026,
-6.70919866065647));
#28400=CARTESIAN_POINT('Ctrl Pts',(-186.041188703775,-92.9007087164244,
-3.99710358616408));
#28401=CARTESIAN_POINT('Ctrl Pts',(-185.718995817204,-93.2976548774544,
-5.05164861453889));
#28402=CARTESIAN_POINT('Ctrl Pts',(-185.831571633446,-93.9828534973759,
-5.99578623488975));
#28403=CARTESIAN_POINT('Ctrl Pts',(-185.725094679122,-93.288633082395,-3.73845962749167));
#28404=CARTESIAN_POINT('Ctrl Pts',(-185.397870201454,-93.6890041414562,
-4.7194370719052));
#28405=CARTESIAN_POINT('Ctrl Pts',(-185.460673954076,-94.3492762075906,
-5.60781290938695));
#28406=CARTESIAN_POINT('Ctrl Pts',(-185.26239384512,-93.8509141779562,-3.29959059468005));
#28407=CARTESIAN_POINT('Ctrl Pts',(-184.927254687052,-94.2568244120627,
-4.15809811654345));
#28408=CARTESIAN_POINT('Ctrl Pts',(-184.917956107225,-94.8794830727165,
-4.94949632679128));
#28409=CARTESIAN_POINT('Ctrl Pts',(-185.110100842455,-94.0350359525012,
-3.14470232541573));
#28410=CARTESIAN_POINT('Ctrl Pts',(-184.772547238992,-94.4425242407308,
-3.96077463262501));
#28411=CARTESIAN_POINT('Ctrl Pts',(-184.739361183769,-95.0529459454586,
-4.7171591757551));
#28412=CARTESIAN_POINT('Ctrl Pts',(-184.811378660606,-94.3944781767998,
-2.81104162227018));
#28413=CARTESIAN_POINT('Ctrl Pts',(-184.469109421573,-94.8050009590216,
-3.53678993922348));
#28414=CARTESIAN_POINT('Ctrl Pts',(-184.389112179675,-95.3912948695953,
-4.21665767553714));
#28415=CARTESIAN_POINT('Ctrl Pts',(-184.665079428327,-94.5696290815887,
-2.63230461390646));
#28416=CARTESIAN_POINT('Ctrl Pts',(-184.320469107015,-94.9816612329742,
-3.31021936162184));
#28417=CARTESIAN_POINT('Ctrl Pts',(-184.217610983093,-95.5560191001983,
-3.94854645547927));
#28418=CARTESIAN_POINT('Ctrl Pts',(-184.388187849506,-94.8997059913566,
-2.2486720114352));
#28419=CARTESIAN_POINT('Ctrl Pts',(-184.039194420781,-95.3145079035315,
-2.82506962104317));
#28420=CARTESIAN_POINT('Ctrl Pts',(-183.893075603405,-95.866206695358,-3.37308506758693));
#28421=CARTESIAN_POINT('Ctrl Pts',(-184.255927894453,-95.0566151233063,
-2.04158414607042));
#28422=CARTESIAN_POINT('Ctrl Pts',(-183.904793548771,-95.4727832060237,
-2.56373454159151));
#28423=CARTESIAN_POINT('Ctrl Pts',(-183.738087091486,-96.0135328517609,
-3.06244641605404));
#28424=CARTESIAN_POINT('Ctrl Pts',(-184.018381326421,-95.337442413618,-1.59313909222305));
#28425=CARTESIAN_POINT('Ctrl Pts',(-183.663477755893,-95.7559537126499,
-1.99898838883818));
#28426=CARTESIAN_POINT('Ctrl Pts',(-183.459757334003,-96.277039469216,-2.38976375451145));
#28427=CARTESIAN_POINT('Ctrl Pts',(-183.913817195825,-95.4605163133078,
-1.35404044643148));
#28428=CARTESIAN_POINT('Ctrl Pts',(-183.557189126045,-95.8801261409614,
-1.69836151638071));
#28429=CARTESIAN_POINT('Ctrl Pts',(-183.337262264464,-96.3924294146135,
-2.03110764218774));
#28430=CARTESIAN_POINT('Ctrl Pts',(-183.790170269781,-95.6057447562368,
-0.961207376336125));
#28431=CARTESIAN_POINT('Ctrl Pts',(-183.431532892932,-96.0266119307892,
-1.20506005246625));
#28432=CARTESIAN_POINT('Ctrl Pts',(-183.192424146606,-96.5285376692198,
-1.44184452599264));
#28433=CARTESIAN_POINT('Ctrl Pts',(-183.754299774836,-95.6478116998946,
-0.822876876377623));
#28434=CARTESIAN_POINT('Ctrl Pts',(-183.395083934597,-96.0690372751092,
-1.03150468099448));
#28435=CARTESIAN_POINT('Ctrl Pts',(-183.150408545955,-96.5679516794309,
-1.23434398753411));
#28436=CARTESIAN_POINT('Ctrl Pts',(-183.69902716988,-95.7125878059592,-0.540441124336129));
#28437=CARTESIAN_POINT('Ctrl Pts',(-183.338932219072,-96.1343505158706,
-0.677342088342398));
#28438=CARTESIAN_POINT('Ctrl Pts',(-183.085668751854,-96.6286349566287,
-0.810680543872514));
#28439=CARTESIAN_POINT('Ctrl Pts',(-183.679493142585,-95.7354542735151,
-0.396620730396645));
#28440=CARTESIAN_POINT('Ctrl Pts',(-183.319081792273,-96.1574129706951,
-0.497048550961574));
#28441=CARTESIAN_POINT('Ctrl Pts',(-183.062789945167,-96.6500520617893,
-0.594944942795723));
#28442=CARTESIAN_POINT('Ctrl Pts',(-183.658485069448,-95.7600444241304,
-0.103191726056088));
#28443=CARTESIAN_POINT('Ctrl Pts',(-183.29773947503,-96.1822068475422,-0.129318689522527));
#28444=CARTESIAN_POINT('Ctrl Pts',(-183.03818476333,-96.6730832760899,-0.154791192776197));
#28445=CARTESIAN_POINT('Ctrl Pts',(-183.657281213906,-95.7614526744861,
0.0472614384620889));
#28446=CARTESIAN_POINT('Ctrl Pts',(-183.296516085829,-96.1836271975658,
0.0592303429672961));
#28447=CARTESIAN_POINT('Ctrl Pts',(-183.036774812679,-96.6744020956455,
0.0708938077874082));
#28448=CARTESIAN_POINT('Ctrl Pts',(-183.673584361532,-95.742371119294,0.340679262059982));
#28449=CARTESIAN_POINT('Ctrl Pts',(-183.313078626216,-96.1643875627615,
0.42693279541692));
#28450=CARTESIAN_POINT('Ctrl Pts',(-183.055869410689,-96.6565304997003,
0.511030789142554));
#28451=CARTESIAN_POINT('Ctrl Pts',(-183.690857386544,-95.722154582619,0.48526389943555));
#28452=CARTESIAN_POINT('Ctrl Pts',(-183.330631578546,-96.1439976105343,
0.608171774735233));
#28453=CARTESIAN_POINT('Ctrl Pts',(-183.076099939953,-96.6375959224396,
0.727912784662916));
#28454=CARTESIAN_POINT('Ctrl Pts',(-183.742255432096,-95.6619321066489,
0.770500979870421));
#28455=CARTESIAN_POINT('Ctrl Pts',(-183.382847157453,-96.0832758362534,
0.96580994111752));
#28456=CARTESIAN_POINT('Ctrl Pts',(-183.136301021943,-96.5811807995018,
1.15577832611497));
#28457=CARTESIAN_POINT('Ctrl Pts',(-183.776157527914,-95.6221850412214,
0.909351028967857));
#28458=CARTESIAN_POINT('Ctrl Pts',(-183.417296348802,-96.0431898175952,
1.1399943994718));
#28459=CARTESIAN_POINT('Ctrl Pts',(-183.176010556326,-96.543942355829,1.36405821104099));
#28460=CARTESIAN_POINT('Ctrl Pts',(-183.855733792922,-95.528750005071,1.17450600394942));
#28461=CARTESIAN_POINT('Ctrl Pts',(-183.498137619005,-95.9489789521239,
1.47279411141771));
#28462=CARTESIAN_POINT('Ctrl Pts',(-183.269223772346,-96.4563802390939,
1.76179982405154));
#28463=CARTESIAN_POINT('Ctrl Pts',(-183.901618838555,-95.4748146345266,
1.30195095812007));
#28464=CARTESIAN_POINT('Ctrl Pts',(-183.544760523303,-95.8945852221131,
1.63286614073801));
#28465=CARTESIAN_POINT('Ctrl Pts',(-183.322974451362,-96.4058247503125,
1.9529716304919));
#28466=CARTESIAN_POINT('Ctrl Pts',(-184.003311269862,-95.3550653583824,
1.54843340014721));
#28467=CARTESIAN_POINT('Ctrl Pts',(-183.648068240509,-95.7738395791422,
1.94266932112714));
#28468=CARTESIAN_POINT('Ctrl Pts',(-183.442107513798,-96.2935423316836,
2.32270370778772));
#28469=CARTESIAN_POINT('Ctrl Pts',(-184.059298282184,-95.2890376172853,
1.66765797594319));
#28470=CARTESIAN_POINT('Ctrl Pts',(-183.704951723409,-95.7072529344379,
2.09265259025143));
#28471=CARTESIAN_POINT('Ctrl Pts',(-183.507700412238,-96.2316144996131,
2.50154461511258));
#28472=CARTESIAN_POINT('Ctrl Pts',(-184.176852645184,-95.1501214463336,
1.89427491600449));
#28473=CARTESIAN_POINT('Ctrl Pts',(-183.824371480539,-95.5671780822467,
2.37798322300348));
#28474=CARTESIAN_POINT('Ctrl Pts',(-183.645434899623,-96.1012760045966,
2.84147765793412));
#28475=CARTESIAN_POINT('Ctrl Pts',(-184.238711432394,-95.0768906699632,
2.00242188310459));
#28476=CARTESIAN_POINT('Ctrl Pts',(-183.887217279107,-95.4933286417111,
2.51428318649114));
#28477=CARTESIAN_POINT('Ctrl Pts',(-183.717917865943,-96.0325444858201,
3.00370172415377));
#28478=CARTESIAN_POINT('Ctrl Pts',(-184.431540341704,-94.8481206782299,
2.31455411749311));
#28479=CARTESIAN_POINT('Ctrl Pts',(-184.083210281331,-95.2625185890143,
2.90827578108584));
#28480=CARTESIAN_POINT('Ctrl Pts',(-183.943883949142,-95.8177457977801,
3.47191039252339));
#28481=CARTESIAN_POINT('Ctrl Pts',(-184.569662566592,-94.6836182645234,
2.50639205885069));
#28482=CARTESIAN_POINT('Ctrl Pts',(-184.223558056762,-95.096589316792,3.15082824084193));
#28483=CARTESIAN_POINT('Ctrl Pts',(-184.10576675548,-95.6631811146341,3.75967355830051));
#28484=CARTESIAN_POINT('Ctrl Pts',(-184.858717524764,-94.3376512020014,
2.86757408695932));
#28485=CARTESIAN_POINT('Ctrl Pts',(-184.517183278251,-94.7477114570037,
3.60852645239219));
#28486=CARTESIAN_POINT('Ctrl Pts',(-184.444611440482,-95.3378252413274,
4.30145816243324));
#28487=CARTESIAN_POINT('Ctrl Pts',(-185.008454788704,-94.1576148308574,
3.03519751519597));
#28488=CARTESIAN_POINT('Ctrl Pts',(-184.669304580449,-94.5661300912731,
3.8214674405414));
#28489=CARTESIAN_POINT('Ctrl Pts',(-184.620171995052,-95.168376829891,4.55289856427253));
#28490=CARTESIAN_POINT('Ctrl Pts',(-185.463984272662,-93.6071208020851,
3.50623173809894));
#28491=CARTESIAN_POINT('Ctrl Pts',(-185.132626075302,-94.010243710356,4.42215777302216));
#28492=CARTESIAN_POINT('Ctrl Pts',(-185.154364647646,-94.6497916478071,
5.25946424297357));
#28493=CARTESIAN_POINT('Ctrl Pts',(-185.777957045331,-93.2240351821244,
3.78096556311151));
#28494=CARTESIAN_POINT('Ctrl Pts',(-185.451626884343,-93.6237620559661,
4.77394349177421));
#28495=CARTESIAN_POINT('Ctrl Pts',(-185.522692219371,-94.2883029853266,
5.67157304213761));
#28496=CARTESIAN_POINT('Ctrl Pts',(-186.415826334264,-92.4372580682707,
4.28435082010938));
#28497=CARTESIAN_POINT('Ctrl Pts',(-186.099491131265,-92.8302396868848,
5.4221694834975));
#28498=CARTESIAN_POINT('Ctrl Pts',(-186.271292454703,-93.5444970023476,
6.42666499108573));
#28499=CARTESIAN_POINT('Ctrl Pts',(-186.739930459906,-92.033330946282,4.51235264699637));
#28500=CARTESIAN_POINT('Ctrl Pts',(-186.428710026573,-92.4227379511592,
5.71753872292767));
#28501=CARTESIAN_POINT('Ctrl Pts',(-186.651807929004,-93.161960330059,6.76867375764101));
#28502=CARTESIAN_POINT('Ctrl Pts',(-187.393530947007,-91.2095920430833,
4.9357741836659));
#28503=CARTESIAN_POINT('Ctrl Pts',(-187.092477352195,-91.5918564120394,
6.26953035299208));
#28504=CARTESIAN_POINT('Ctrl Pts',(-187.419481988969,-92.3803984155784,
7.40381660388869));
#28505=CARTESIAN_POINT('Ctrl Pts',(-187.723431876917,-90.789245324442,5.13113846604913));
#28506=CARTESIAN_POINT('Ctrl Pts',(-187.427506580947,-91.1677963691818,
6.52589394947526));
#28507=CARTESIAN_POINT('Ctrl Pts',(-187.807116502426,-91.9808618362968,
7.69686757472972));
#28508=CARTESIAN_POINT('Ctrl Pts',(-188.379735239133,-89.9434589515106,
5.49397424411016));
#28509=CARTESIAN_POINT('Ctrl Pts',(-188.093936031686,-90.3146004408659,
7.00530187354627));
#28510=CARTESIAN_POINT('Ctrl Pts',(-188.578584928303,-91.1754925110962,
8.24112908982782));
#28511=CARTESIAN_POINT('Ctrl Pts',(-188.707031074314,-89.5169094143503,
5.66196658593984));
#28512=CARTESIAN_POINT('Ctrl Pts',(-188.426255795464,-89.8842722210176,
7.22884474588428));
#28513=CARTESIAN_POINT('Ctrl Pts',(-188.963467607895,-90.7686092384922,
8.49312094838692));
#28514=CARTESIAN_POINT('Ctrl Pts',(-189.68511297814,-88.2275681149711,6.13501898387808));
#28515=CARTESIAN_POINT('Ctrl Pts',(-189.422317700218,-88.5795741093693,
7.86491570906493));
#28516=CARTESIAN_POINT('Ctrl Pts',(-190.114092759895,-89.5365583941309,
9.20270785472519));
#28517=CARTESIAN_POINT('Ctrl Pts',(-190.332033957746,-87.3551470887722,
6.40961295144101));
#28518=CARTESIAN_POINT('Ctrl Pts',(-190.078977721377,-87.6992096958193,
8.23877620276131));
#28519=CARTESIAN_POINT('Ctrl Pts',(-190.875743827135,-88.7000469473906,
9.61460278261497));
#28520=CARTESIAN_POINT('Ctrl Pts',(-191.611898320755,-85.5882580977726,
6.90461427888993));
#28521=CARTESIAN_POINT('Ctrl Pts',(-191.378062267531,-85.9164296154525,
8.92407374163879));
#28522=CARTESIAN_POINT('Ctrl Pts',(-192.383730616602,-87.0002198715461,
10.3571100610023));
#28523=CARTESIAN_POINT('Ctrl Pts',(-192.244891171766,-84.693736712425,7.12463735632059));
#28524=CARTESIAN_POINT('Ctrl Pts',(-192.020340574275,-85.0137142395017,
9.23418963052937));
#28525=CARTESIAN_POINT('Ctrl Pts',(-193.130124103834,-86.1368550460551,
10.6871461172942));
#28526=CARTESIAN_POINT('Ctrl Pts',(-194.119961067917,-81.9797996678922,
7.72418030763564));
#28527=CARTESIAN_POINT('Ctrl Pts',(-193.934940664567,-82.257849756744,10.1010557721888));
#28528=CARTESIAN_POINT('Ctrl Pts',(-195.342719172301,-83.50920211737,11.5864611755336));
#28529=CARTESIAN_POINT('Ctrl Pts',(-195.338006413608,-80.1301500968197,
8.04415647990219));
#28530=CARTESIAN_POINT('Ctrl Pts',(-195.16935199361,-80.3905659076323,10.5812896754235));
#28531=CARTESIAN_POINT('Ctrl Pts',(-196.782194293857,-81.7074776699032,
12.0664230083597));
#28532=CARTESIAN_POINT('Ctrl Pts',(-197.110239250038,-77.3006000230673,
8.44922123457134));
#28533=CARTESIAN_POINT('Ctrl Pts',(-196.954831995167,-77.5532375792707,
11.2157823096582));
#28534=CARTESIAN_POINT('Ctrl Pts',(-198.879361941047,-78.935681607343,12.6740132502263));
#28535=CARTESIAN_POINT('Ctrl Pts',(-197.692624677484,-76.3469248856778,
8.5715135010636));
#28536=CARTESIAN_POINT('Ctrl Pts',(-197.544944403591,-76.5909251985067,
11.414061030348));
#28537=CARTESIAN_POINT('Ctrl Pts',(-199.569000827311,-77.9989242812487,
12.8574486612482));
#28538=CARTESIAN_POINT('Ctrl Pts',(-198.833501317186,-74.43002371175,8.79383680878653));
#28539=CARTESIAN_POINT('Ctrl Pts',(-198.701046000336,-74.6567602970987,
11.7854080990333));
#28540=CARTESIAN_POINT('Ctrl Pts',(-200.920841970448,-76.1111237379196,
13.1909267424754));
#28541=CARTESIAN_POINT('Ctrl Pts',(-199.392274367538,-73.4664233641185,
8.89394683892845));
#28542=CARTESIAN_POINT('Ctrl Pts',(-199.266893542384,-73.6846080389232,
11.9582237199827));
#28543=CARTESIAN_POINT('Ctrl Pts',(-201.583376310003,-75.1597219207058,
13.3410879530753));
#28544=CARTESIAN_POINT('Ctrl Pts',(-201.033783983709,-70.5604287764574,
9.16677201385106));
#28545=CARTESIAN_POINT('Ctrl Pts',(-200.940109283218,-70.7339672756153,
12.4488343143003));
#28546=CARTESIAN_POINT('Ctrl Pts',(-203.530870313903,-72.2835771071226,
13.7503128604518));
#28547=CARTESIAN_POINT('Ctrl Pts',(-202.081723044656,-68.6028539641832,
9.31223534268044));
#28548=CARTESIAN_POINT('Ctrl Pts',(-201.999085118096,-68.7598621453509,
12.7310897529191));
#28549=CARTESIAN_POINT('Ctrl Pts',(-204.775735293809,-70.3369061379169,
13.9684983839894));
#28550=CARTESIAN_POINT('Ctrl Pts',(-204.085562846173,-64.6481906295588,
9.55122215804647));
#28551=CARTESIAN_POINT('Ctrl Pts',(-204.026314097882,-64.7713562775311,
13.238108357264));
#28552=CARTESIAN_POINT('Ctrl Pts',(-207.158618873108,-66.387628113296,14.3269579904162));
#28553=CARTESIAN_POINT('Ctrl Pts',(-205.041466127102,-62.6510984859536,
9.64459843558729));
#28554=CARTESIAN_POINT('Ctrl Pts',(-204.990809880274,-62.7587308992531,
13.4607910313532));
#28555=CARTESIAN_POINT('Ctrl Pts',(-208.296641479989,-64.3850167536084,
14.4670115183672));
#28556=CARTESIAN_POINT('Ctrl Pts',(-207.771662686836,-56.601430798315,9.86749344214829));
#28557=CARTESIAN_POINT('Ctrl Pts',(-207.783522326383,-56.5847268119357,
14.0716577550469));
#28558=CARTESIAN_POINT('Ctrl Pts',(-211.550002283707,-58.2963858291117,
14.8013197394809));
#28559=CARTESIAN_POINT('Ctrl Pts',(-209.408693149567,-52.4905952748467,
9.94066884240314));
#28560=CARTESIAN_POINT('Ctrl Pts',(-209.420079879466,-52.454626832127,14.3810813496773));
#28561=CARTESIAN_POINT('Ctrl Pts',(-213.504906168685,-54.1297053236517,
14.9110597099366));
#28562=CARTESIAN_POINT('Ctrl Pts',(-212.31378134909,-44.1146587717776,10.0094381670403));
#28563=CARTESIAN_POINT('Ctrl Pts',(-212.345419819919,-44.0267219078386,
14.9024839573744));
#28564=CARTESIAN_POINT('Ctrl Pts',(-216.978639285811,-45.5934511118201,
15.0141686414793));
#28565=CARTESIAN_POINT('Ctrl Pts',(-213.581879775254,-39.8495543519757,
10.0043954519828));
#28566=CARTESIAN_POINT('Ctrl Pts',(-213.605139445775,-39.7586824716392,
15.1062312896536));
#28567=CARTESIAN_POINT('Ctrl Pts',(-218.497528523746,-41.2238500697657,
15.0065832746786));
#28568=CARTESIAN_POINT('Ctrl Pts',(-214.929428919574,-34.4198302895606,
9.97920576186122));
#28569=CARTESIAN_POINT('Ctrl Pts',(-214.936859859468,-34.3891593318107,
15.3153703026194));
#28570=CARTESIAN_POINT('Ctrl Pts',(-220.113030275332,-35.6397174849627,
14.9687749372571));
#28571=CARTESIAN_POINT('Ctrl Pts',(-215.187043011382,-33.3287590530146,
9.97318130845427));
#28572=CARTESIAN_POINT('Ctrl Pts',(-215.19468682512,-33.2957346146807,15.3553818376476));
#28573=CARTESIAN_POINT('Ctrl Pts',(-220.421957075912,-34.5165678200411,
14.9597336598784));
#28574=CARTESIAN_POINT('Ctrl Pts',(-215.675983586131,-31.1472549362169,
9.95985565385693));
#28575=CARTESIAN_POINT('Ctrl Pts',(-215.68418616737,-31.1095679945434,15.4307038587473));
#28576=CARTESIAN_POINT('Ctrl Pts',(-221.008423709188,-32.2690261896159,
14.9397363624086));
#28577=CARTESIAN_POINT('Ctrl Pts',(-215.90764622814,-30.055516718288,9.95254907226967));
#28578=CARTESIAN_POINT('Ctrl Pts',(-215.915775634413,-30.0163642711029,
15.4659963578014));
#28579=CARTESIAN_POINT('Ctrl Pts',(-221.286366523007,-31.1432926323065,
14.9287722668472));
#28580=CARTESIAN_POINT('Ctrl Pts',(-216.564558495436,-26.7773677629292,
9.92956539341713));
#28581=CARTESIAN_POINT('Ctrl Pts',(-216.575423316015,-26.7202845042959,
15.5658559264057));
#28582=CARTESIAN_POINT('Ctrl Pts',(-222.074674899071,-27.7605386096942,
14.8942846816766));
#28583=CARTESIAN_POINT('Ctrl Pts',(-216.951752658587,-24.5880241878653,
9.91285560896527));
#28584=CARTESIAN_POINT('Ctrl Pts',(-216.960777488742,-24.5333219085994,
15.6232654891544));
#28585=CARTESIAN_POINT('Ctrl Pts',(-222.539542982626,-25.4979652324832,
14.8692127365989));
#28586=CARTESIAN_POINT('Ctrl Pts',(-217.963118570905,-18.0083995826229,
9.86431151401665));
#28587=CARTESIAN_POINT('Ctrl Pts',(-217.976908530276,-17.9105064968268,
15.7736929532904));
#28588=CARTESIAN_POINT('Ctrl Pts',(-223.754139848201,-18.6905621049579,
14.7963774439254));
#28589=CARTESIAN_POINT('Ctrl Pts',(-218.43737553185,-13.6065465446901,9.83453026560912));
#28590=CARTESIAN_POINT('Ctrl Pts',(-218.441702505744,-13.5485089098786,
15.8411776329903));
#28591=CARTESIAN_POINT('Ctrl Pts',(-224.324191182824,-14.1260707926592,
14.7516962153847));
#28592=CARTESIAN_POINT('Ctrl Pts',(-218.989193202051,-4.7721628047025,9.79912404537101));
#28593=CARTESIAN_POINT('Ctrl Pts',(-218.990897585228,-4.7335129665023,15.9210896224386));
#28594=CARTESIAN_POINT('Ctrl Pts',(-224.987517064859,-4.95696670963562,
14.6985760232229));
#28595=CARTESIAN_POINT('Ctrl Pts',(-219.066759730313,-0.339632492972661,
9.79351850252103));
#28596=CARTESIAN_POINT('Ctrl Pts',(-219.066727564461,-0.350430413971326,
15.9320679979825));
#28597=CARTESIAN_POINT('Ctrl Pts',(-225.080801055053,-0.352320764338334,
14.6901661447284));
#28598=CARTESIAN_POINT('Ctrl Pts',(-218.880718901755,6.33255501405285,9.8059454221472));
#28599=CARTESIAN_POINT('Ctrl Pts',(-218.881432931089,6.31289977575216,15.9051486662368));
#28600=CARTESIAN_POINT('Ctrl Pts',(-224.857132572439,6.57614298146129,14.7088102047727));
#28601=CARTESIAN_POINT('Ctrl Pts',(-218.768230359849,8.56052172271425,9.81343805284001));
#28602=CARTESIAN_POINT('Ctrl Pts',(-218.770003081734,8.53077447021609,15.8889618235594));
#28603=CARTESIAN_POINT('Ctrl Pts',(-224.721894016949,8.88921878827596,14.7200513807027));
#28604=CARTESIAN_POINT('Ctrl Pts',(-218.522448524829,11.9084288001204,9.82890166451567));
#28605=CARTESIAN_POINT('Ctrl Pts',(-218.524928042834,11.8774402237096,15.8532704560566));
#28606=CARTESIAN_POINT('Ctrl Pts',(-224.426467103965,12.3631418548612,14.7432516194942));
#28607=CARTESIAN_POINT('Ctrl Pts',(-218.427625255158,13.0254701659967,9.83475451805377));
#28608=CARTESIAN_POINT('Ctrl Pts',(-218.430609970526,12.991870685901,15.8395230780581));
#28609=CARTESIAN_POINT('Ctrl Pts',(-224.312498386649,13.5219155099691,14.7520327570961));
#28610=CARTESIAN_POINT('Ctrl Pts',(-218.21323860133,15.2503993161315,9.84754794127491));
#28611=CARTESIAN_POINT('Ctrl Pts',(-218.217068753284,15.2132620015528,15.8083419032611));
#28612=CARTESIAN_POINT('Ctrl Pts',(-224.054856092527,15.8291500128444,14.7712270705584));
#28613=CARTESIAN_POINT('Ctrl Pts',(-218.093583727244,16.3596870431594,9.85449428714121));
#28614=CARTESIAN_POINT('Ctrl Pts',(-218.097966645082,16.3205496369381,15.7909263232461));
#28615=CARTESIAN_POINT('Ctrl Pts',(-223.911072517391,16.979063905479,14.7816489139371));
#28616=CARTESIAN_POINT('Ctrl Pts',(-217.433606562207,21.8903944208552,9.89118647408106));
#28617=CARTESIAN_POINT('Ctrl Pts',(-217.445236527621,21.8024400591546,15.6952267122392));
#28618=CARTESIAN_POINT('Ctrl Pts',(-223.118121902026,22.7098222865059,14.8366999810007));
#28619=CARTESIAN_POINT('Ctrl Pts',(-216.708563916788,26.2647200848804,9.92732876816586));
#28620=CARTESIAN_POINT('Ctrl Pts',(-216.731935048167,26.1494884159972,15.5904394521733));
#28621=CARTESIAN_POINT('Ctrl Pts',(-222.247281590068,27.2343164729745,14.8909272767638));
#28622=CARTESIAN_POINT('Ctrl Pts',(-214.873442978039,34.9151616307584,9.98467680865938));
#28623=CARTESIAN_POINT('Ctrl Pts',(-214.895229142084,34.8173622853258,15.310263695862));
#28624=CARTESIAN_POINT('Ctrl Pts',(-220.045590647228,36.1539662505485,14.9769827670247));
#28625=CARTESIAN_POINT('Ctrl Pts',(-213.763346868112,39.1912731419991,10.0059888635648));
#28626=CARTESIAN_POINT('Ctrl Pts',(-213.795786303056,39.0868620241777,15.1393495471316));
#28627=CARTESIAN_POINT('Ctrl Pts',(-218.71471064539,40.5491477077801,15.0089703691583));
#28628=CARTESIAN_POINT('Ctrl Pts',(-211.157664540089,47.6451012812898,9.99106655001459));
#28629=CARTESIAN_POINT('Ctrl Pts',(-211.176219821159,47.5841008473432,14.6986672737439));
#28630=CARTESIAN_POINT('Ctrl Pts',(-215.595563893305,49.1983243309679,14.9866296990289));
#28631=CARTESIAN_POINT('Ctrl Pts',(-209.662098742207,51.8228239014422,9.95531537582467));
#28632=CARTESIAN_POINT('Ctrl Pts',(-209.685532101084,51.7729467688604,14.4360702739088));
#28633=CARTESIAN_POINT('Ctrl Pts',(-213.80730640242,53.4523572352619,14.9330257980933));
#28634=CARTESIAN_POINT('Ctrl Pts',(-207.545508834274,56.9818337014807,9.83445365866236));
#28635=CARTESIAN_POINT('Ctrl Pts',(-207.510723871588,57.0648634396861,14.0005580141263));
#28636=CARTESIAN_POINT('Ctrl Pts',(-211.281520603173,58.6720114070539,14.7517626507157));
#28637=CARTESIAN_POINT('Ctrl Pts',(-207.109809764703,58.0104721219209,9.80639282881937));
#28638=CARTESIAN_POINT('Ctrl Pts',(-207.071261697803,58.1008397078743,13.9102924731027));
#28639=CARTESIAN_POINT('Ctrl Pts',(-210.761813438706,59.7110402643347,14.7096772084586));
#28640=CARTESIAN_POINT('Ctrl Pts',(-206.213392812189,60.0613541485855,9.74108338571072));
#28641=CARTESIAN_POINT('Ctrl Pts',(-206.166184591471,60.1672120878568,13.7184889746833));
#28642=CARTESIAN_POINT('Ctrl Pts',(-209.693081442639,61.7790036523918,14.6117245857318));
#28643=CARTESIAN_POINT('Ctrl Pts',(-205.752839497752,61.08313643902,9.70383665509273));
#28644=CARTESIAN_POINT('Ctrl Pts',(-205.701230510568,61.1968025962474,13.6171538768307));
#28645=CARTESIAN_POINT('Ctrl Pts',(-209.144253544922,62.8074679437847,14.5558602053489));
#28646=CARTESIAN_POINT('Ctrl Pts',(-204.339722003525,64.1253772453607,9.57651965325937));
#28647=CARTESIAN_POINT('Ctrl Pts',(-204.282123111009,64.2443553233843,13.2971569314029));
#28648=CARTESIAN_POINT('Ctrl Pts',(-207.461156573031,65.8638453333561,14.3649014156848));
#28649=CARTESIAN_POINT('Ctrl Pts',(-203.353817729955,66.1271301231815,9.47090861847069));
#28650=CARTESIAN_POINT('Ctrl Pts',(-203.286815403105,66.2623803486336,13.0595360566483));
#28651=CARTESIAN_POINT('Ctrl Pts',(-206.288029158072,67.867179527562,14.2064955657256));
#28652=CARTESIAN_POINT('Ctrl Pts',(-201.295982075669,70.0773663077491,9.20351075942536));
#28653=CARTESIAN_POINT('Ctrl Pts',(-201.204273063212,70.2469450403615,12.51897904355));
#28654=CARTESIAN_POINT('Ctrl Pts',(-203.84229300212,71.8036809549284,13.8054187109848));
#28655=CARTESIAN_POINT('Ctrl Pts',(-200.224040052249,72.0258588331287,9.04188770997817));
#28656=CARTESIAN_POINT('Ctrl Pts',(-200.12047497987,72.2124872803002,12.2182147537059));
#28657=CARTESIAN_POINT('Ctrl Pts',(-202.569671040505,73.7368570614262,13.5629930900514));
#28658=CARTESIAN_POINT('Ctrl Pts',(-197.995685176027,75.8684360666186,8.64078280222561));
#28659=CARTESIAN_POINT('Ctrl Pts',(-197.862702838989,76.0899116945249,11.5260954437677));
#28660=CARTESIAN_POINT('Ctrl Pts',(-199.927578782646,77.5306853270276,12.9613510241432));
#28661=CARTESIAN_POINT('Ctrl Pts',(-196.839245861665,77.7625466240603,8.40173977014487));
#28662=CARTESIAN_POINT('Ctrl Pts',(-196.691996019402,78.0013102762491,11.1379598928392));
#28663=CARTESIAN_POINT('Ctrl Pts',(-198.558076797564,79.3913614209033,12.60279242272));
#28664=CARTESIAN_POINT('Ctrl Pts',(-195.042731573518,80.5611850737664,7.95715194188054));
#28665=CARTESIAN_POINT('Ctrl Pts',(-194.858551738376,80.8435039704777,10.4503583874007));
#28666=CARTESIAN_POINT('Ctrl Pts',(-196.433609218416,82.125363186609,11.9359168266832));
#28667=CARTESIAN_POINT('Ctrl Pts',(-194.433589268338,81.4869661634149,7.79447520514001));
#28668=CARTESIAN_POINT('Ctrl Pts',(-194.240902692785,81.7777231153474,10.2062460954892));
#28669=CARTESIAN_POINT('Ctrl Pts',(-195.713756493118,83.0271859261819,11.6919029300314));
#28670=CARTESIAN_POINT('Ctrl Pts',(-193.195101021216,83.3238217818029,7.43221244759254));
#28671=CARTESIAN_POINT('Ctrl Pts',(-192.984483082209,83.6312855291968,9.67471802243613));
#28672=CARTESIAN_POINT('Ctrl Pts',(-194.251251280249,84.8111598877124,11.1485096657566));
#28673=CARTESIAN_POINT('Ctrl Pts',(-192.565602902613,84.2350179279496,7.23258583606902));
#28674=CARTESIAN_POINT('Ctrl Pts',(-192.345875521816,84.5508501176059,9.38782701439113));
#28675=CARTESIAN_POINT('Ctrl Pts',(-193.508421789667,85.6934162800533,10.8490693154141));
#28676=CARTESIAN_POINT('Ctrl Pts',(-191.295766122429,86.0299410528198,6.78753527123933));
#28677=CARTESIAN_POINT('Ctrl Pts',(-191.057182564862,86.3619994488762,8.76050448431005));
#28678=CARTESIAN_POINT('Ctrl Pts',(-192.011112251812,87.4258398244962,10.1814905385105));
#28679=CARTESIAN_POINT('Ctrl Pts',(-190.654477805639,86.9150843481393,6.54205946398291));
#28680=CARTESIAN_POINT('Ctrl Pts',(-190.406326530197,87.25527815843,8.42065139010884));
#28681=CARTESIAN_POINT('Ctrl Pts',(-191.255510732542,88.2773832319173,9.81327421990134));
#28682=CARTESIAN_POINT('Ctrl Pts',(-189.349584768406,88.6752321827888,5.98095856523893));
#28683=CARTESIAN_POINT('Ctrl Pts',(-189.081798171609,89.0309342903906,7.65676092118989));
#28684=CARTESIAN_POINT('Ctrl Pts',(-189.719216239347,89.9651010967815,8.97161470628148));
#28685=CARTESIAN_POINT('Ctrl Pts',(-188.685650085394,89.5498148663974,5.66466085148541));
#28686=CARTESIAN_POINT('Ctrl Pts',(-188.407635601515,89.9135939257602,7.23283181006476));
#28687=CARTESIAN_POINT('Ctrl Pts',(-188.93805424261,90.8008600150856,8.49708749073966));
#28688=CARTESIAN_POINT('Ctrl Pts',(-188.020722526437,90.4061090473696,5.2954583188303));
#28689=CARTESIAN_POINT('Ctrl Pts',(-187.728390752002,90.7825752206079,6.74229702851374));
#28690=CARTESIAN_POINT('Ctrl Pts',(-188.15658149337,91.6160251236586,7.94335562892809));
#28691=CARTESIAN_POINT('',(-188.06083509298,90.3544283086146,5.31766757924143));
#28692=CARTESIAN_POINT('',(-188.311118109849,-90.0308913574651,-5.4533811546917));
#28693=CARTESIAN_POINT('Ctrl Pts',(-188.06083509298,90.3544283086146,5.31766757924145));
#28694=CARTESIAN_POINT('Ctrl Pts',(-188.51680197023,89.7666938435659,5.56940638867454));
#28695=CARTESIAN_POINT('Ctrl Pts',(-188.972498711518,89.1700935523622,5.79657748555383));
#28696=CARTESIAN_POINT('Ctrl Pts',(-189.426627535133,88.5659108843427,6.00556125304925));
#28697=CARTESIAN_POINT('Ctrl Pts',(-189.619911580624,88.3087616698077,6.09450788211784));
#28698=CARTESIAN_POINT('Ctrl Pts',(-189.81291152598,88.050239085108,6.18016056957736));
#28699=CARTESIAN_POINT('Ctrl Pts',(-190.00552702852,87.7904427618453,6.26301392151901));
#28700=CARTESIAN_POINT('Ctrl Pts',(-190.0065706244,87.7890351785042,6.26346282316814));
#28701=CARTESIAN_POINT('Ctrl Pts',(-190.007614208963,87.7876275578147,6.26391164261233));
#28702=CARTESIAN_POINT('Ctrl Pts',(-190.008657782195,87.7862198997925,6.26436037993047));
#28703=CARTESIAN_POINT('Ctrl Pts',(-190.573087725994,87.0248700354609,6.50706570388179));
#28704=CARTESIAN_POINT('Ctrl Pts',(-191.13430700821,86.2524813601324,6.72525538225101));
#28705=CARTESIAN_POINT('Ctrl Pts',(-191.691014022882,85.4702469629432,6.9250607165503));
#28706=CARTESIAN_POINT('Ctrl Pts',(-191.769609740418,85.359811361975,6.95326916947602));
#28707=CARTESIAN_POINT('Ctrl Pts',(-191.848115518518,85.249179541194,6.98111127249217));
#28708=CARTESIAN_POINT('Ctrl Pts',(-191.926527692939,85.1383548791639,7.00860435543439));
#28709=CARTESIAN_POINT('Ctrl Pts',(-191.92791329294,85.1363965269951,7.00909017815311));
#28710=CARTESIAN_POINT('Ctrl Pts',(-191.929298863927,85.1344381143097,7.00957589192428));
#28711=CARTESIAN_POINT('Ctrl Pts',(-191.930684405876,85.1324796411284,7.01006149684292));
#28712=CARTESIAN_POINT('Ctrl Pts',(-192.487088704112,84.3459982959562,7.20507014607013));
#28713=CARTESIAN_POINT('Ctrl Pts',(-193.039539566412,83.5486706128072,7.3825606229965));
#28714=CARTESIAN_POINT('Ctrl Pts',(-193.584625019812,82.7450778439038,7.5454311084043));
#28715=CARTESIAN_POINT('Ctrl Pts',(-193.660087593468,82.6338270700391,7.56797918031646));
#28716=CARTESIAN_POINT('Ctrl Pts',(-193.735409008233,82.5224562631648,7.59024711098675));
#28717=CARTESIAN_POINT('Ctrl Pts',(-193.810580221864,82.4109776165522,7.61224265150016));
#28718=CARTESIAN_POINT('Ctrl Pts',(-193.81183523018,82.4091164436146,7.61260987433606));
#28719=CARTESIAN_POINT('Ctrl Pts',(-193.813090196661,82.4072552405714,7.61297702124396));
#28720=CARTESIAN_POINT('Ctrl Pts',(-193.814345121268,82.4053940074768,7.6133440922604));
#28721=CARTESIAN_POINT('Ctrl Pts',(-194.432553090273,81.4885029645941,7.79417266663633));
#28722=CARTESIAN_POINT('Ctrl Pts',(-195.040750453091,80.5641977261954,7.95662373930324));
#28723=CARTESIAN_POINT('Ctrl Pts',(-195.638717557925,79.6327484802435,8.10464224532399));
#28724=CARTESIAN_POINT('Ctrl Pts',(-195.639668281456,79.6312675447386,8.10487758381603));
#28725=CARTESIAN_POINT('Ctrl Pts',(-195.640618979127,79.6297865911748,8.10511288582298));
#28726=CARTESIAN_POINT('Ctrl Pts',(-195.641569650937,79.6283056195534,8.1053481513607));
#28727=CARTESIAN_POINT('Ctrl Pts',(-196.838915668809,77.763061004687,8.40165887801138));
#28728=CARTESIAN_POINT('Ctrl Pts',(-197.99521745823,75.8692128806453,8.64068943479255));
#28729=CARTESIAN_POINT('Ctrl Pts',(-199.109366290497,73.9480033042068,8.84124604920835));
#28730=CARTESIAN_POINT('Ctrl Pts',(-199.109531730703,73.947718023373,8.84127582990427));
#28731=CARTESIAN_POINT('Ctrl Pts',(-199.109697169979,73.9474327419359,8.84130560975191));
#28732=CARTESIAN_POINT('Ctrl Pts',(-199.109862608326,73.9471474598955,8.84133538875136));
#28733=CARTESIAN_POINT('Ctrl Pts',(-200.223942142281,72.026027669517,9.04187035788895));
#28734=CARTESIAN_POINT('Ctrl Pts',(-201.29590104568,70.0775218531977,9.20350054478848));
#28735=CARTESIAN_POINT('Ctrl Pts',(-202.324899898542,68.1022482236617,9.33720984811441));
#28736=CARTESIAN_POINT('Ctrl Pts',(-202.325616587401,68.1008724625512,9.33730297549529));
#28737=CARTESIAN_POINT('Ctrl Pts',(-202.326333255426,68.0994966884513,9.33739608925299));
#28738=CARTESIAN_POINT('Ctrl Pts',(-202.327049902617,68.0981209013622,9.33748918939001));
#28739=CARTESIAN_POINT('Ctrl Pts',(-203.355125526122,66.1244674934296,9.47104721167366));
#28740=CARTESIAN_POINT('Ctrl Pts',(-204.340330517151,64.1240672021237,9.57657447788188));
#28741=CARTESIAN_POINT('Ctrl Pts',(-205.28180033275,62.0972167083591,9.66139767126757));
#28742=CARTESIAN_POINT('Ctrl Pts',(-205.283387201231,62.0938004064126,9.66154064266165));
#28743=CARTESIAN_POINT('Ctrl Pts',(-205.284973950805,62.0903840168381,9.66168355513634));
#28744=CARTESIAN_POINT('Ctrl Pts',(-205.286560581401,62.0869675397905,9.66182640871456));
#28745=CARTESIAN_POINT('Ctrl Pts',(-205.755928257212,61.0762824471217,9.70408630975619));
#28746=CARTESIAN_POINT('Ctrl Pts',(-206.214896939989,60.0579129054442,9.74119304854463));
#28747=CARTESIAN_POINT('Ctrl Pts',(-206.661601287996,59.0359131362846,9.77373814714519));
#28748=CARTESIAN_POINT('Ctrl Pts',(-206.663590354042,59.031362419351,9.77388306257059));
#28749=CARTESIAN_POINT('Ctrl Pts',(-206.66557917369,59.0268116395308,9.7740278875185));
#28750=CARTESIAN_POINT('Ctrl Pts',(-206.667567746947,59.0222607968317,9.77417262205041));
#28751=CARTESIAN_POINT('Ctrl Pts',(-207.113676431887,58.0013426866808,9.8066417963464));
#28752=CARTESIAN_POINT('Ctrl Pts',(-207.547387284822,56.9772551360114,9.83456186917772));
#28753=CARTESIAN_POINT('Ctrl Pts',(-207.968826809702,55.9500317564852,9.85862677614977));
#28754=CARTESIAN_POINT('Ctrl Pts',(-207.971163590813,55.9443360491565,9.85876021028857));
#28755=CARTESIAN_POINT('Ctrl Pts',(-207.973499995396,55.9386402456129,9.85889352833538));
#28756=CARTESIAN_POINT('Ctrl Pts',(-207.975836023462,55.9329443458578,9.85902673037562));
#28757=CARTESIAN_POINT('Ctrl Pts',(-209.666224089052,51.8112982462088,9.95541390241721));
#28758=CARTESIAN_POINT('Ctrl Pts',(-211.159461284655,47.6392719557561,9.99108029052597));
#28759=CARTESIAN_POINT('Ctrl Pts',(-212.460505703252,43.4181872143984,9.99852947308981));
#28760=CARTESIAN_POINT('Ctrl Pts',(-212.463715926966,43.4077720232338,9.99854785335583));
#28761=CARTESIAN_POINT('Ctrl Pts',(-212.466924980455,43.3973565333573,9.99856605889622));
#28762=CARTESIAN_POINT('Ctrl Pts',(-212.470132863722,43.3869407447705,9.99858409003113));
#28763=CARTESIAN_POINT('Ctrl Pts',(-213.768815578448,39.1702023323294,10.0058838329716));
#28764=CARTESIAN_POINT('Ctrl Pts',(-214.875703511897,34.9045058683299,9.9846099748668));
#28765=CARTESIAN_POINT('Ctrl Pts',(-215.791003449954,30.589940845844,9.95600474013346));
#28766=CARTESIAN_POINT('Ctrl Pts',(-215.794260322957,30.5745885118635,9.95590295533826));
#28767=CARTESIAN_POINT('Ctrl Pts',(-215.797514770452,30.559235559204,9.95580107637761));
#28768=CARTESIAN_POINT('Ctrl Pts',(-215.800766792235,30.5438819878149,9.95569910388854));
#28769=CARTESIAN_POINT('Ctrl Pts',(-216.713708471003,26.2336663211255,9.92707231675218));
#28770=CARTESIAN_POINT('Ctrl Pts',(-217.435480651459,21.8746892726661,9.8910825901607));
#28771=CARTESIAN_POINT('Ctrl Pts',(-217.961588294286,17.4658285182826,9.86183279026221));
#28772=CARTESIAN_POINT('Ctrl Pts',(-217.964035693427,17.445318947339,9.86169672317379));
#28773=CARTESIAN_POINT('Ctrl Pts',(-217.966478850021,17.4248082947604,9.86156079087027));
#28774=CARTESIAN_POINT('Ctrl Pts',(-217.968917763295,17.4042965603517,9.86142499435562));
#28775=CARTESIAN_POINT('Ctrl Pts',(-218.098016566448,16.318550547643,9.85423688820197));
#28776=CARTESIAN_POINT('Ctrl Pts',(-218.215230776192,15.2297242981946,9.84742921466242));
#28777=CARTESIAN_POINT('Ctrl Pts',(-218.320431928289,14.1379347405934,9.84115131508478));
#28778=CARTESIAN_POINT('Ctrl Pts',(-218.322535801835,14.1161005009297,9.84102576601444));
#28779=CARTESIAN_POINT('Ctrl Pts',(-218.324634906511,14.0942645369404,9.84090042657939));
#28780=CARTESIAN_POINT('Ctrl Pts',(-218.326729238281,14.0724268925217,9.84077529794832));
#28781=CARTESIAN_POINT('Ctrl Pts',(-218.431337469398,12.981674516305,9.83452534034928));
#28782=CARTESIAN_POINT('Ctrl Pts',(-218.524056391673,11.8865273086927,9.82880091068774));
#28783=CARTESIAN_POINT('Ctrl Pts',(-218.604375803264,10.7924597730254,9.82374741828564));
#28784=CARTESIAN_POINT('Ctrl Pts',(-218.606072766715,10.7693446557215,9.82364064967597));
#28785=CARTESIAN_POINT('Ctrl Pts',(-218.60776421916,10.7462299863214,9.82353418301963));
#28786=CARTESIAN_POINT('Ctrl Pts',(-218.609450161518,10.7231157661814,9.82342801890493));
#28787=CARTESIAN_POINT('Ctrl Pts',(-218.770554963031,8.51437367592111,9.81328321855358));
#28788=CARTESIAN_POINT('Ctrl Pts',(-218.881361170861,6.30952061087333,9.80590609607315));
#28789=CARTESIAN_POINT('Ctrl Pts',(-218.942732511399,4.10849250724635,9.80180559598378));
#28790=CARTESIAN_POINT('Ctrl Pts',(-218.94344205954,4.08304519935568,9.80175818782569));
#28791=CARTESIAN_POINT('Ctrl Pts',(-218.94414500976,4.05759840202034,9.80171123365064));
#28792=CARTESIAN_POINT('Ctrl Pts',(-218.944841362669,4.03215211519381,9.80166473310975));
#28793=CARTESIAN_POINT('Ctrl Pts',(-219.065865799387,-0.390350456036404,
9.79358305254647));
#28794=CARTESIAN_POINT('Ctrl Pts',(-218.987614587639,-4.79743579236434,
9.7992336121286));
#28795=CARTESIAN_POINT('Ctrl Pts',(-218.713284367982,-9.18935465820405,
9.81683142676904));
#28796=CARTESIAN_POINT('Ctrl Pts',(-218.711406729688,-9.21941490843551,
9.81695187405592));
#28797=CARTESIAN_POINT('Ctrl Pts',(-218.709519905522,-9.24947444815586,
9.81707288013222));
#28798=CARTESIAN_POINT('Ctrl Pts',(-218.70762389497,-9.27953327733394,9.81719444199773));
#28799=CARTESIAN_POINT('Ctrl Pts',(-218.430911254125,-13.666459284364,9.8349357487566));
#28800=CARTESIAN_POINT('Ctrl Pts',(-217.95852998986,-18.0382514286823,9.86453422912174));
#28801=CARTESIAN_POINT('Ctrl Pts',(-217.288874630294,-22.3948159800386,
9.89667511604252));
#28802=CARTESIAN_POINT('Ctrl Pts',(-217.283555754183,-22.4294188944924,
9.89693040168043));
#28803=CARTESIAN_POINT('Ctrl Pts',(-217.278224413937,-22.4640208469283,
9.89718581860337));
#28804=CARTESIAN_POINT('Ctrl Pts',(-217.272880606905,-22.4986218371657,
9.89744135928248));
#28805=CARTESIAN_POINT('Ctrl Pts',(-216.939522261105,-24.6571071266348,
9.91338254457614));
#28806=CARTESIAN_POINT('Ctrl Pts',(-216.557648993695,-26.8118478251854,
9.92980747149138));
#28807=CARTESIAN_POINT('Ctrl Pts',(-216.126616984069,-28.9628003990182,
9.94488797127757));
#28808=CARTESIAN_POINT('Ctrl Pts',(-216.119233106746,-28.9996477086767,
9.94514631069991));
#28809=CARTESIAN_POINT('Ctrl Pts',(-216.111834797523,-29.0364939062531,
9.94540424670578));
#28810=CARTESIAN_POINT('Ctrl Pts',(-216.104422051958,-29.0733389914415,
9.9456617682015));
#28811=CARTESIAN_POINT('Ctrl Pts',(-215.892008213258,-30.1291429326299,
9.95304110275137));
#28812=CARTESIAN_POINT('Ctrl Pts',(-215.667723636287,-31.1841083198772,
9.96008078617996));
#28813=CARTESIAN_POINT('Ctrl Pts',(-215.431513298767,-32.2380069945684,
9.96651848957129));
#28814=CARTESIAN_POINT('Ctrl Pts',(-215.423005023906,-32.2759683289206,
9.96675037506158));
#28815=CARTESIAN_POINT('Ctrl Pts',(-215.414480871154,-32.3139298605291,
9.96698148614846));
#28816=CARTESIAN_POINT('Ctrl Pts',(-215.40594089593,-32.3518913495086,9.96721180811115));
#28817=CARTESIAN_POINT('Ctrl Pts',(-215.16911597409,-33.4046141530769,9.97359894383225));
#28818=CARTESIAN_POINT('Ctrl Pts',(-214.920050029317,-34.457620960072,9.97938362263439));
#28819=CARTESIAN_POINT('Ctrl Pts',(-214.659919093045,-35.5057750926369,
9.98424592547359));
#28820=CARTESIAN_POINT('Ctrl Pts',(-214.650247074172,-35.5447468762224,
9.98442671244765));
#28821=CARTESIAN_POINT('Ctrl Pts',(-214.64055978287,-35.5837122211703,9.9846062788195));
#28822=CARTESIAN_POINT('Ctrl Pts',(-214.630857226511,-35.622671116418,9.98478460672069));
#28823=CARTESIAN_POINT('Ctrl Pts',(-213.559099608934,-39.9261238571264,
10.0044829500703));
#28824=CARTESIAN_POINT('Ctrl Pts',(-212.300728554187,-44.1522925375462,
10.0091555454261));
#28825=CARTESIAN_POINT('Ctrl Pts',(-210.861237215767,-48.302627120132,9.97506716298549));
#28826=CARTESIAN_POINT('Ctrl Pts',(-210.846648861139,-48.3446881948322,
9.97472169830747));
#28827=CARTESIAN_POINT('Ctrl Pts',(-210.832041900486,-48.386741481317,9.97437231709957));
#28828=CARTESIAN_POINT('Ctrl Pts',(-210.817416335251,-48.4287869789396,
9.97401898219888));
#28829=CARTESIAN_POINT('Ctrl Pts',(-209.375759165835,-52.5732553885937,
9.93919039372426));
#28830=CARTESIAN_POINT('Ctrl Pts',(-207.753330793897,-56.642051284793,9.86601251598906));
#28831=CARTESIAN_POINT('Ctrl Pts',(-205.951531538682,-60.6345428301356,
9.71890487965252));
#28832=CARTESIAN_POINT('Ctrl Pts',(-205.931370267354,-60.6792168997281,
9.71725881560739));
#28833=CARTESIAN_POINT('Ctrl Pts',(-205.91118650737,-60.7238813995598,9.71560338632713));
#28834=CARTESIAN_POINT('Ctrl Pts',(-205.890980256884,-60.7685363263265,
9.71393851524477));
#28835=CARTESIAN_POINT('Ctrl Pts',(-204.999073030556,-62.7396121526445,
9.64045083130972));
#28836=CARTESIAN_POINT('Ctrl Pts',(-204.063345493926,-64.6920375334682,
9.54857804243365));
#28837=CARTESIAN_POINT('Ctrl Pts',(-203.083642786703,-66.6255226101039,
9.43173548532964));
#28838=CARTESIAN_POINT('Ctrl Pts',(-202.081695627481,-68.6029080614775,
9.31223998194527));
#28839=CARTESIAN_POINT('Ctrl Pts',(-201.033751116317,-70.5604869697111,
9.16677491688292));
#28840=CARTESIAN_POINT('Ctrl Pts',(-199.939444119453,-72.4977587142569,
8.98489165361757));
#28841=CARTESIAN_POINT('Ctrl Pts',(-199.91309919235,-72.5443976218348,8.98051289946019));
#28842=CARTESIAN_POINT('Ctrl Pts',(-199.88672738753,-72.5910247522546,8.97611289164215));
#28843=CARTESIAN_POINT('Ctrl Pts',(-199.860328698315,-72.6376400958351,
8.97169142002573));
#28844=CARTESIAN_POINT('Ctrl Pts',(-199.338431354915,-73.5592170642366,
8.88427972046174));
#28845=CARTESIAN_POINT('Ctrl Pts',(-198.806014126144,-74.4762076967677,
8.78848127769314));
#28846=CARTESIAN_POINT('Ctrl Pts',(-198.263062970022,-75.3884743446064,
8.68267570895607));
#28847=CARTESIAN_POINT('Ctrl Pts',(-198.235092082578,-75.4354710356309,
8.67722498724615));
#28848=CARTESIAN_POINT('Ctrl Pts',(-198.207092562445,-75.4824560900013,
8.67174751883111));
#28849=CARTESIAN_POINT('Ctrl Pts',(-198.179064838505,-75.5294288251994,
8.66624311624193));
#28850=CARTESIAN_POINT('Ctrl Pts',(-197.635470254205,-76.4404597928872,
8.55948584106465));
#28851=CARTESIAN_POINT('Ctrl Pts',(-197.08120557516,-77.3469552823971,8.44262055412659));
#28852=CARTESIAN_POINT('Ctrl Pts',(-196.519493300536,-78.2437860485531,
8.31422647338811));
#28853=CARTESIAN_POINT('Ctrl Pts',(-196.490056260816,-78.2907852758758,
8.30749786547763));
#28854=CARTESIAN_POINT('Ctrl Pts',(-196.460596833056,-78.3377612230074,
8.30073821556141));
#28855=CARTESIAN_POINT('Ctrl Pts',(-196.431115108733,-78.3847138039004,
8.29394705947406));
#28856=CARTESIAN_POINT('Ctrl Pts',(-195.695048802598,-79.5569726718873,
8.1243931649728));
#28857=CARTESIAN_POINT('Ctrl Pts',(-194.945007563397,-80.7147865676449,
7.9352916044913));
#28858=CARTESIAN_POINT('Ctrl Pts',(-194.182159059277,-81.8572132916295,
7.71947409973443));
#28859=CARTESIAN_POINT('Ctrl Pts',(-193.748804736262,-82.5061960934465,
7.59687380863673));
#28860=CARTESIAN_POINT('Ctrl Pts',(-193.311317539902,-83.1502134702393,
7.46565285377205));
#28861=CARTESIAN_POINT('Ctrl Pts',(-192.869912506659,-83.7890938733829,
7.32450466033796));
#28862=CARTESIAN_POINT('Ctrl Pts',(-192.838362656537,-83.8347584658703,
7.31441595719134));
#28863=CARTESIAN_POINT('Ctrl Pts',(-192.80679286958,-83.8803967263716,7.304275914378));
#28864=CARTESIAN_POINT('Ctrl Pts',(-192.775203283695,-83.9260085284507,
7.29408359580739));
#28865=CARTESIAN_POINT('Ctrl Pts',(-192.266915439948,-84.6599188941247,
7.13008550960481));
#28866=CARTESIAN_POINT('Ctrl Pts',(-191.753495353972,-85.3869876622751,
6.95261874682967));
#28867=CARTESIAN_POINT('Ctrl Pts',(-191.235538330077,-86.1066609025267,
6.75770746303479));
#28868=CARTESIAN_POINT('Ctrl Pts',(-191.147808666634,-86.2285565198139,
6.72469410374118));
#28869=CARTESIAN_POINT('Ctrl Pts',(-191.059948858487,-86.3502399712669,
6.69118041028271));
#28870=CARTESIAN_POINT('Ctrl Pts',(-190.971961813689,-86.4717085650345,
6.65714721763566));
#28871=CARTESIAN_POINT('Ctrl Pts',(-190.939875691232,-86.5160043608901,
6.64473637704678));
#28872=CARTESIAN_POINT('Ctrl Pts',(-190.90777252411,-86.560271718568,6.63225741831689));
#28873=CARTESIAN_POINT('Ctrl Pts',(-190.875652557489,-86.6045103960844,
6.61970860958682));
#28874=CARTESIAN_POINT('Ctrl Pts',(-190.401447417493,-87.2576308838022,
6.43444348553252));
#28875=CARTESIAN_POINT('Ctrl Pts',(-189.923571498165,-87.9045121020593,
6.23403435388213));
#28876=CARTESIAN_POINT('Ctrl Pts',(-189.442826746467,-88.5443600219234,
6.01293258678423));
#28877=CARTESIAN_POINT('Ctrl Pts',(-189.306461275911,-88.725855841416,5.95021604873683));
#28878=CARTESIAN_POINT('Ctrl Pts',(-189.169864992924,-88.9067857888991,
5.88583489329034));
#28879=CARTESIAN_POINT('Ctrl Pts',(-189.033056229673,-89.0871318100725,
5.8196632777581));
#28880=CARTESIAN_POINT('Ctrl Pts',(-189.001009116442,-89.1293774179127,
5.80416274105795));
#28881=CARTESIAN_POINT('Ctrl Pts',(-188.96895048776,-89.1715908315416,5.78856285244983));
#28882=CARTESIAN_POINT('Ctrl Pts',(-188.936880751009,-89.2137716331804,
5.77286066138358));
#28883=CARTESIAN_POINT('Ctrl Pts',(-188.683433073572,-89.547127229166,5.64876597712418));
#28884=CARTESIAN_POINT('Ctrl Pts',(-188.429224761621,-89.8785325446022,
5.51826779476947));
#28885=CARTESIAN_POINT('Ctrl Pts',(-188.174626035996,-90.2075623578002,
5.37998727999571));
#28886=CARTESIAN_POINT('Ctrl Pts',(-188.133621029437,-90.2605550411505,
5.35771618102844));
#28887=CARTESIAN_POINT('Ctrl Pts',(-188.092605902664,-90.313486129659,5.33524331946663));
#28888=CARTESIAN_POINT('Ctrl Pts',(-188.05158220932,-90.3663538760784,5.31256306641583));
#28889=CARTESIAN_POINT('Ctrl Pts',(-188.019880255481,-90.4072085802729,
5.29503640617024));
#28890=CARTESIAN_POINT('Ctrl Pts',(-187.988164848065,-90.4480358164431,
5.27738103636211));
#28891=CARTESIAN_POINT('Ctrl Pts',(-187.956440707941,-90.4888298148183,
5.259595025775));
#28892=CARTESIAN_POINT('Ctrl Pts',(-187.75306131691,-90.7503549031177,5.14557119446294));
#28893=CARTESIAN_POINT('Ctrl Pts',(-187.549103864686,-91.0107947425876,
5.02608364485494));
#28894=CARTESIAN_POINT('Ctrl Pts',(-187.345892263011,-91.268521005334,4.90062671379455));
#28895=CARTESIAN_POINT('Ctrl Pts',(-187.25263651765,-91.386794049459,4.84305332959621));
#28896=CARTESIAN_POINT('Ctrl Pts',(-187.159537867347,-91.5044957625111,
4.78422344319158));
#28897=CARTESIAN_POINT('Ctrl Pts',(-187.066723847658,-91.6214701352587,
4.72409173688634));
#28898=CARTESIAN_POINT('Ctrl Pts',(-187.035938485457,-91.6602692137318,
4.70414672895975));
#28899=CARTESIAN_POINT('Ctrl Pts',(-187.005180842154,-91.6989930300589,
4.68405900940515));
#28900=CARTESIAN_POINT('Ctrl Pts',(-186.974453572332,-91.7376387068004,
4.66382280836529));
#28901=CARTESIAN_POINT('Ctrl Pts',(-186.781298812858,-91.9805693817015,
4.53661597979979));
#28902=CARTESIAN_POINT('Ctrl Pts',(-186.589254838546,-92.2205246511467,
4.40358022722448));
#28903=CARTESIAN_POINT('Ctrl Pts',(-186.398878611342,-92.4569161279226,
4.26313874687862));
#28904=CARTESIAN_POINT('Ctrl Pts',(-186.297709583587,-92.582538408742,4.18850585688057));
#28905=CARTESIAN_POINT('Ctrl Pts',(-186.197011499421,-92.7071543463695,
4.11178235875304));
#28906=CARTESIAN_POINT('Ctrl Pts',(-186.096867627569,-92.8306763058842,
4.03273768018468));
#28907=CARTESIAN_POINT('Ctrl Pts',(-186.068151779818,-92.8660957251426,
4.01007194025181));
#28908=CARTESIAN_POINT('Ctrl Pts',(-186.039479816593,-92.9014271072812,
3.98722064024348));
#28909=CARTESIAN_POINT('Ctrl Pts',(-186.010855777804,-92.9366660656645,
3.96417195795104));
#28910=CARTESIAN_POINT('Ctrl Pts',(-185.865981518665,-93.1150202813691,
3.84751613604557));
#28911=CARTESIAN_POINT('Ctrl Pts',(-185.722265707347,-93.2910917770091,
3.72582451668043));
#28912=CARTESIAN_POINT('Ctrl Pts',(-185.580307265502,-93.4642190437351,
3.59764267842825));
#28913=CARTESIAN_POINT('Ctrl Pts',(-185.450978642463,-93.6219434504375,
3.48086497627492));
#28914=CARTESIAN_POINT('Ctrl Pts',(-185.323108761286,-93.7772240998859,
3.35870017216342));
#28915=CARTESIAN_POINT('Ctrl Pts',(-185.197140819223,-93.9295753497621,
3.23009067295042));
#28916=CARTESIAN_POINT('Ctrl Pts',(-185.184839193751,-93.944453484512,3.21753108147375));
#28917=CARTESIAN_POINT('Ctrl Pts',(-185.172555697486,-93.9593036951516,
3.20491006625581));
#28918=CARTESIAN_POINT('Ctrl Pts',(-185.160290736874,-93.9741255382158,
3.19222666815781));
#28919=CARTESIAN_POINT('Ctrl Pts',(-185.135032506227,-94.0046493647953,
3.16610671517324));
#28920=CARTESIAN_POINT('Ctrl Pts',(-185.109840003889,-94.0350683943748,
3.13970033206727));
#28921=CARTESIAN_POINT('Ctrl Pts',(-185.084727989822,-94.0653655712933,
3.11299775843998));
#28922=CARTESIAN_POINT('Ctrl Pts',(-185.000757625597,-94.1666742506354,
3.02370882975576));
#28923=CARTESIAN_POINT('Ctrl Pts',(-184.917546304095,-94.2667902418731,
2.93098623593855));
#28924=CARTESIAN_POINT('Ctrl Pts',(-184.835738044685,-94.3649633720747,
2.83451960455793));
#28925=CARTESIAN_POINT('Ctrl Pts',(-184.794841327897,-94.4140410413836,
2.78629503002805));
#28926=CARTESIAN_POINT('Ctrl Pts',(-184.754295103115,-94.4626333930311,
2.73713544658652));
#28927=CARTESIAN_POINT('Ctrl Pts',(-184.714178396369,-94.5106486763438,
2.68700652086778));
#28928=CARTESIAN_POINT('Ctrl Pts',(-184.691560089061,-94.5377203011496,
2.65874319770587));
#28929=CARTESIAN_POINT('Ctrl Pts',(-184.669107579012,-94.5645735297545,
2.63021393443707));
#28930=CARTESIAN_POINT('Ctrl Pts',(-184.646834983318,-94.5911925894902,
2.60140281589878));
#28931=CARTESIAN_POINT('Ctrl Pts',(-184.558200755562,-94.697123655435,2.48674840931461));
#28932=CARTESIAN_POINT('Ctrl Pts',(-184.472336938954,-94.7994405101602,
2.36757759974578));
#28933=CARTESIAN_POINT('Ctrl Pts',(-184.39001361699,-94.8972907412225,2.24276030558802));
#28934=CARTESIAN_POINT('Ctrl Pts',(-184.360538666391,-94.9323249290794,
2.19807086046513));
#28935=CARTESIAN_POINT('Ctrl Pts',(-184.331517390034,-94.966786755673,2.15265794738168));
#28936=CARTESIAN_POINT('Ctrl Pts',(-184.302984457013,-95.0006378956154,
2.10647100277846));
#28937=CARTESIAN_POINT('Ctrl Pts',(-184.284616631745,-95.0224292699243,
2.07673856246047));
#28938=CARTESIAN_POINT('Ctrl Pts',(-184.266453222769,-95.0439652433064,
2.04668207816586));
#28939=CARTESIAN_POINT('Ctrl Pts',(-184.248509638701,-95.0652285217695,
2.01627815072083));
#28940=CARTESIAN_POINT('Ctrl Pts',(-184.203571054875,-95.1184810725424,
1.94013341637187));
#28941=CARTESIAN_POINT('Ctrl Pts',(-184.160013235404,-95.1700208923274,
1.86181972998249));
#28942=CARTESIAN_POINT('Ctrl Pts',(-184.11807248382,-95.2195830531759,1.78097027598704));
#28943=CARTESIAN_POINT('Ctrl Pts',(-184.065729691486,-95.2814374977177,
1.68006874177653));
#28944=CARTESIAN_POINT('Ctrl Pts',(-184.015676542522,-95.3404806834878,
1.57462166859957));
#28945=CARTESIAN_POINT('Ctrl Pts',(-183.969546039874,-95.3948223314433,
1.46600813692336));
#28946=CARTESIAN_POINT('Ctrl Pts',(-183.963788790444,-95.4016043607678,
1.45245278509672));
#28947=CARTESIAN_POINT('Ctrl Pts',(-183.958092599144,-95.4083132066439,
1.43884808896023));
#28948=CARTESIAN_POINT('Ctrl Pts',(-183.952460605122,-95.4149452355462,
1.42519670863897));
#28949=CARTESIAN_POINT('Ctrl Pts',(-183.939870672291,-95.4297706771367,
1.39467999277968));
#28950=CARTESIAN_POINT('Ctrl Pts',(-183.92759053512,-95.4442253572866,1.36391850743349));
#28951=CARTESIAN_POINT('Ctrl Pts',(-183.91563674564,-95.4582906918077,1.33289908442677));
#28952=CARTESIAN_POINT('Ctrl Pts',(-183.888000177376,-95.4908090474554,
1.26118371727321));
#28953=CARTESIAN_POINT('Ctrl Pts',(-183.862086334608,-95.521271749357,1.18803365022812));
#28954=CARTESIAN_POINT('Ctrl Pts',(-183.838139395079,-95.5494024579498,
1.11341655287846));
#28955=CARTESIAN_POINT('Ctrl Pts',(-183.830539615712,-95.5583299945345,
1.08973613742647));
#28956=CARTESIAN_POINT('Ctrl Pts',(-183.823137717431,-95.5670229192437,
1.06590814401409));
#28957=CARTESIAN_POINT('Ctrl Pts',(-183.815940854834,-95.5754731656678,
1.04193206334385));
#28958=CARTESIAN_POINT('Ctrl Pts',(-183.807052112064,-95.5859099449995,
1.01231954666276));
#28959=CARTESIAN_POINT('Ctrl Pts',(-183.798465657636,-95.5959888299654,
0.982424266488826));
#28960=CARTESIAN_POINT('Ctrl Pts',(-183.790207377758,-95.6056800572553,
0.952284262991848));
#28961=CARTESIAN_POINT('Ctrl Pts',(-183.770637055188,-95.6286461527345,
0.880859026811543));
#28962=CARTESIAN_POINT('Ctrl Pts',(-183.752834291628,-95.6495237102342,
0.807724319669422));
#28963=CARTESIAN_POINT('Ctrl Pts',(-183.737174261358,-95.667880389908,0.733396237962366));
#28964=CARTESIAN_POINT('Ctrl Pts',(-183.729815806035,-95.6765059675685,
0.698470387944005));
#28965=CARTESIAN_POINT('Ctrl Pts',(-183.722930052581,-95.6845754234538,
0.663281346768663));
#28966=CARTESIAN_POINT('Ctrl Pts',(-183.716553371217,-95.6920469043472,
0.627883782731233));
#28967=CARTESIAN_POINT('Ctrl Pts',(-183.711527814294,-95.6979352889768,
0.599986438821077));
#28968=CARTESIAN_POINT('Ctrl Pts',(-183.706826946361,-95.7034423959074,
0.57202855141883));
#28969=CARTESIAN_POINT('Ctrl Pts',(-183.702455562656,-95.7085628613754,
0.544016869547344));
#28970=CARTESIAN_POINT('Ctrl Pts',(-183.690432620339,-95.7226460590806,
0.466974253730033));
#28971=CARTESIAN_POINT('Ctrl Pts',(-183.680879377209,-95.7338310775459,
0.389326927627816));
#28972=CARTESIAN_POINT('Ctrl Pts',(-183.673906168774,-95.7419938810966,
0.311176583107222));
#28973=CARTESIAN_POINT('Ctrl Pts',(-183.670430979897,-95.7460619201294,
0.272229345192594));
#28974=CARTESIAN_POINT('Ctrl Pts',(-183.667596074987,-95.7493799400455,
0.233157230799864));
#28975=CARTESIAN_POINT('Ctrl Pts',(-183.665411948407,-95.7519362878294,
0.193973187426416));
#28976=CARTESIAN_POINT('Ctrl Pts',(-183.664060507716,-95.7535180424976,
0.169727838683484));
#28977=CARTESIAN_POINT('Ctrl Pts',(-183.662964569235,-95.7548007725713,
0.145395417202572));
#28978=CARTESIAN_POINT('Ctrl Pts',(-183.662122791516,-95.7557860370457,
0.121013577556789));
#28979=CARTESIAN_POINT('Ctrl Pts',(-183.659349263018,-95.7590323323995,
0.0406791548507267));
#28980=CARTESIAN_POINT('Ctrl Pts',(-183.659369903306,-95.7590083849867,
-0.0405743786132426));
#28981=CARTESIAN_POINT('Ctrl Pts',(-183.662167137276,-95.7557343635116,
-0.121409031646972));
#28982=CARTESIAN_POINT('Ctrl Pts',(-183.66365575411,-95.7539920124849,-0.164427179750673));
#28983=CARTESIAN_POINT('Ctrl Pts',(-183.665930163209,-95.7513298702821,
-0.20732660630546));
#28984=CARTESIAN_POINT('Ctrl Pts',(-183.668983873669,-95.7477554733448,
-0.249907146204909));
#28985=CARTESIAN_POINT('Ctrl Pts',(-183.67039589183,-95.7461026927514,-0.269596143044668));
#28986=CARTESIAN_POINT('Ctrl Pts',(-183.671969627319,-95.7442605895704,
-0.289232202416622));
#28987=CARTESIAN_POINT('Ctrl Pts',(-183.673702142494,-95.7422325155245,
-0.308814502605387));
#28988=CARTESIAN_POINT('Ctrl Pts',(-183.683157232174,-95.7311644323959,
-0.415683641223018));
#28989=CARTESIAN_POINT('Ctrl Pts',(-183.697388129984,-95.7145027257029,
-0.521069269126041));
#28990=CARTESIAN_POINT('Ctrl Pts',(-183.716065692174,-95.6926183979358,
-0.625191032757183));
#28991=CARTESIAN_POINT('Ctrl Pts',(-183.719449769401,-95.6886533057849,
-0.64405624041201));
#28992=CARTESIAN_POINT('Ctrl Pts',(-183.722979909019,-95.6845166626267,
-0.66287994147631));
#28993=CARTESIAN_POINT('Ctrl Pts',(-183.726654266742,-95.680210541379,-0.681663421242707));
#28994=CARTESIAN_POINT('Ctrl Pts',(-183.729553586093,-95.6768127174321,
-0.696484870450501));
#28995=CARTESIAN_POINT('Ctrl Pts',(-183.732544154011,-95.6733076374794,
-0.711278140450021));
#28996=CARTESIAN_POINT('Ctrl Pts',(-183.735622809827,-95.6696989480456,
-0.726038309658969));
#28997=CARTESIAN_POINT('Ctrl Pts',(-183.754762108044,-95.6472645522066,
-0.817798901629893));
#28998=CARTESIAN_POINT('Ctrl Pts',(-183.777288708933,-95.6208459470195,
-0.908128526296283));
#28999=CARTESIAN_POINT('Ctrl Pts',(-183.802436490926,-95.5913270514141,
-0.995898950364328));
#29000=CARTESIAN_POINT('Ctrl Pts',(-183.811736072317,-95.5804110440969,
-1.02835621448973));
#29001=CARTESIAN_POINT('Ctrl Pts',(-183.821394374083,-95.5690707476792,
-1.06046321037403));
#29002=CARTESIAN_POINT('Ctrl Pts',(-183.831373372734,-95.5573500029804,
-1.09216144311939));
#29003=CARTESIAN_POINT('Ctrl Pts',(-183.834612567923,-95.5535454348907,
-1.10245072830553));
#29004=CARTESIAN_POINT('Ctrl Pts',(-183.837886716341,-95.5496994128863,
-1.11270736160523));
#29005=CARTESIAN_POINT('Ctrl Pts',(-183.84119544588,-95.5458123496254,-1.12293200011363));
#29006=CARTESIAN_POINT('Ctrl Pts',(-183.884539221333,-95.4948925040621,
-1.2568729675859));
#29007=CARTESIAN_POINT('Ctrl Pts',(-183.933756424313,-95.4370013790296,
-1.38512586819768));
#29008=CARTESIAN_POINT('Ctrl Pts',(-183.987818272335,-95.3732923838696,
-1.50869724720684));
#29009=CARTESIAN_POINT('Ctrl Pts',(-184.034246838454,-95.3185788029926,
-1.61482092130545));
#29010=CARTESIAN_POINT('Ctrl Pts',(-184.084247981211,-95.259574924401,-1.71749225159379));
#29011=CARTESIAN_POINT('Ctrl Pts',(-184.13715259088,-95.1970311559832,-1.81736427105629));
#29012=CARTESIAN_POINT('Ctrl Pts',(-184.139376756947,-95.1944017494282,
-1.82156299699304));
#29013=CARTESIAN_POINT('Ctrl Pts',(-184.141605799135,-95.1917663849156,
-1.82575598533418));
#29014=CARTESIAN_POINT('Ctrl Pts',(-184.143839671123,-95.1891251153873,
-1.82994324507604));
#29015=CARTESIAN_POINT('Ctrl Pts',(-184.220435087611,-95.098560776594,-1.97351678265353));
#29016=CARTESIAN_POINT('Ctrl Pts',(-184.302651756358,-95.0011215960924,
-2.11025363025844));
#29017=CARTESIAN_POINT('Ctrl Pts',(-184.388592842741,-94.898977142677,-2.24059233765731));
#29018=CARTESIAN_POINT('Ctrl Pts',(-184.433674618534,-94.8453956307228,
-2.30896359791739));
#29019=CARTESIAN_POINT('Ctrl Pts',(-184.479780684922,-94.7905200050719,
-2.37557437687181));
#29020=CARTESIAN_POINT('Ctrl Pts',(-184.526633468334,-94.73466773982,-2.4404886208611));
#29021=CARTESIAN_POINT('Ctrl Pts',(-184.527176884216,-94.7340199446255,
-2.44124152023089));
#29022=CARTESIAN_POINT('Ctrl Pts',(-184.527720426209,-94.7333719875324,
-2.44199422515958));
#29023=CARTESIAN_POINT('Ctrl Pts',(-184.528264094033,-94.7327238688657,
-2.44274673570745));
#29024=CARTESIAN_POINT('Ctrl Pts',(-184.612107889473,-94.6327717905154,
-2.55879800396048));
#29025=CARTESIAN_POINT('Ctrl Pts',(-184.69886411786,-94.5290729414887,-2.67012237576756));
#29026=CARTESIAN_POINT('Ctrl Pts',(-184.787618496314,-94.4226767227031,
-2.77711763958086));
#29027=CARTESIAN_POINT('Ctrl Pts',(-184.843651702179,-94.3555057128406,
-2.84466684389354));
#29028=CARTESIAN_POINT('Ctrl Pts',(-184.90048179645,-94.2872589546782,-2.91048943974378));
#29029=CARTESIAN_POINT('Ctrl Pts',(-184.957878667389,-94.2181996013897,
-2.9746750548167));
#29030=CARTESIAN_POINT('Ctrl Pts',(-184.958832137028,-94.2170523960528,
-2.97574129822416));
#29031=CARTESIAN_POINT('Ctrl Pts',(-184.959785764468,-94.2159049647762,
-2.9768070912445));
#29032=CARTESIAN_POINT('Ctrl Pts',(-184.960739548435,-94.2147573090282,
-2.97787243402948));
#29033=CARTESIAN_POINT('Ctrl Pts',(-185.055656879252,-94.1005465190806,
-3.08389171833809));
#29034=CARTESIAN_POINT('Ctrl Pts',(-185.152073064151,-93.9841796856407,
-3.18543351709792));
#29035=CARTESIAN_POINT('Ctrl Pts',(-185.249698961493,-93.8659730207856,
-3.28323031733737));
#29036=CARTESIAN_POINT('Ctrl Pts',(-185.303685810653,-93.8006050645476,
-3.33731167532267));
#29037=CARTESIAN_POINT('Ctrl Pts',(-185.358042346536,-93.734674788487,-3.39024870455163));
#29038=CARTESIAN_POINT('Ctrl Pts',(-185.412717994685,-93.6682377807508,
-3.44217144691258));
#29039=CARTESIAN_POINT('Ctrl Pts',(-185.414020826092,-93.6666546953517,
-3.44340868107037));
#29040=CARTESIAN_POINT('Ctrl Pts',(-185.415323838326,-93.6650713226774,
-3.44464533868886));
#29041=CARTESIAN_POINT('Ctrl Pts',(-185.41662703075,-93.6634876634248,-3.44588142160717));
#29042=CARTESIAN_POINT('Ctrl Pts',(-185.541105647225,-93.5122193555825,
-3.56394985779942));
#29043=CARTESIAN_POINT('Ctrl Pts',(-185.667207249309,-93.358359529924,-3.6768454970486));
#29044=CARTESIAN_POINT('Ctrl Pts',(-185.794631041937,-93.20222798354,-3.78530063865651));
#29045=CARTESIAN_POINT('Ctrl Pts',(-185.824114143369,-93.1661025306417,
-3.81039480572569));
#29046=CARTESIAN_POINT('Ctrl Pts',(-185.853667976554,-93.1298555283609,
-3.83525145044411));
#29047=CARTESIAN_POINT('Ctrl Pts',(-185.883288723287,-93.0934910595899,
-3.85988000049324));
#29048=CARTESIAN_POINT('Ctrl Pts',(-185.946688598849,-93.0156570057842,
-3.91259464075803));
#29049=CARTESIAN_POINT('Ctrl Pts',(-186.010647756309,-92.936973960331,-3.96446937120499));
#29050=CARTESIAN_POINT('Ctrl Pts',(-186.074793299048,-92.8578933698295,
-4.01531677064043));
#29051=CARTESIAN_POINT('Ctrl Pts',(-186.144322045734,-92.7721762005619,
-4.070431371032));
#29052=CARTESIAN_POINT('Ctrl Pts',(-186.214069607494,-92.6859919969263,
-4.12433927420305));
#29053=CARTESIAN_POINT('Ctrl Pts',(-186.283549979849,-92.5999389434393,
-4.17685870024448));
#29054=CARTESIAN_POINT('Ctrl Pts',(-186.309404272347,-92.5679178022194,
-4.19640166693666));
#29055=CARTESIAN_POINT('Ctrl Pts',(-186.335221478964,-92.5359150334324,
-4.21575288020181));
#29056=CARTESIAN_POINT('Ctrl Pts',(-186.360976297731,-92.5039621495615,
-4.23490456548554));
#29057=CARTESIAN_POINT('Ctrl Pts',(-186.362273299024,-92.5023530164482,
-4.23586903589422));
#29058=CARTESIAN_POINT('Ctrl Pts',(-186.363570144303,-92.5007440073944,
-4.23683299281394));
#29059=CARTESIAN_POINT('Ctrl Pts',(-186.364866830462,-92.4991351263001,
-4.23779643485467));
#29060=CARTESIAN_POINT('Ctrl Pts',(-186.592435857374,-92.2167757422467,
-4.40688096332591));
#29061=CARTESIAN_POINT('Ctrl Pts',(-186.821641388606,-91.9302462495062,
-4.56497378064983));
#29062=CARTESIAN_POINT('Ctrl Pts',(-187.051828931819,-91.6402373813893,
-4.71444402500823));
#29063=CARTESIAN_POINT('Ctrl Pts',(-187.144372893419,-91.5236430202006,
-4.77453662759256));
#29064=CARTESIAN_POINT('Ctrl Pts',(-187.237075726216,-91.4064860720515,
-4.83323496705587));
#29065=CARTESIAN_POINT('Ctrl Pts',(-187.3298954364,-91.2888106578876,-4.89069088055909));
#29066=CARTESIAN_POINT('Ctrl Pts',(-187.601053998392,-90.9450399649696,
-5.05853952878842));
#29067=CARTESIAN_POINT('Ctrl Pts',(-187.873240567925,-90.5968104926114,
-5.21569175079462));
#29068=CARTESIAN_POINT('Ctrl Pts',(-188.145873603651,-90.2447077922517,
-5.36433722168423));
#29069=CARTESIAN_POINT('Ctrl Pts',(-188.200938440812,-90.1735921337697,
-5.39435977059362));
#29070=CARTESIAN_POINT('Ctrl Pts',(-188.256021524338,-90.1023184107007,
-5.4240351428556));
#29071=CARTESIAN_POINT('Ctrl Pts',(-188.311118109849,-90.0308913574651,
-5.4533811546917));
#29072=CARTESIAN_POINT('Origin',(-192.01137155147,93.4192711577907,5.31766757925036));
#29073=CARTESIAN_POINT('Origin',(-192.27014422543,-93.0847597593693,-5.4533811546917));
#29074=CARTESIAN_POINT('Origin',(0.,-222.,0.));
#29075=CARTESIAN_POINT('',(199.738310248729,-222.,15.));
#29076=CARTESIAN_POINT('Origin',(199.738310248729,-222.,0.));
#29077=CARTESIAN_POINT('',(0.,-222.,15.));
#29078=CARTESIAN_POINT('Origin',(199.738310248729,222.,0.));
#29079=CARTESIAN_POINT('',(199.738310248729,222.,-15.));
#29080=CARTESIAN_POINT('',(199.738310248729,222.,-15.));
#29081=CARTESIAN_POINT('Origin',(199.738310248729,222.,0.));
#29082=CARTESIAN_POINT('Origin',(199.738310248729,-222.,0.));
#29083=CARTESIAN_POINT('Origin',(199.738310248729,222.,0.));
#29084=CARTESIAN_POINT('Origin',(-71.5953323638214,6.93889390390723E-15,
-26.5));
#29085=CARTESIAN_POINT('Ctrl Pts',(-188.311118109849,-90.0308913574651,
-5.4533811546917));
#29086=CARTESIAN_POINT('Ctrl Pts',(-188.753305639072,-89.4576407304613,
-5.68890283719888));
#29087=CARTESIAN_POINT('Ctrl Pts',(-189.193308928458,-88.8784819227758,
-5.90197859397969));
#29088=CARTESIAN_POINT('Ctrl Pts',(-189.63044941269,-88.2940948432694,-6.09829027438424));
#29089=CARTESIAN_POINT('Ctrl Pts',(-189.839578220121,-88.0145229952629,
-6.19220614145355));
#29090=CARTESIAN_POINT('Ctrl Pts',(-190.0480523925,-87.7337550679739,-6.2822852426851));
#29091=CARTESIAN_POINT('Ctrl Pts',(-190.255800837365,-87.4518682623278,
-6.36914968955112));
#29092=CARTESIAN_POINT('Ctrl Pts',(-190.782415688894,-86.7373224644024,
-6.58933958228109));
#29093=CARTESIAN_POINT('Ctrl Pts',(-191.30440717723,-86.0155284126311,-6.78845317883935));
#29094=CARTESIAN_POINT('Ctrl Pts',(-191.821164100696,-85.2870765363022,
-6.97149374860157));
#29095=CARTESIAN_POINT('Ctrl Pts',(-191.934392805452,-85.1274624920808,
-7.011600510003));
#29096=CARTESIAN_POINT('Ctrl Pts',(-192.047370341996,-84.9675289311489,
-7.05093558981425));
#29097=CARTESIAN_POINT('Ctrl Pts',(-192.16009053274,-84.8072822852053,-7.0895516218191));
#29098=CARTESIAN_POINT('Ctrl Pts',(-192.807135210935,-83.8874227749251,
-7.31121819137361));
#29099=CARTESIAN_POINT('Ctrl Pts',(-193.445667235945,-82.9572868867053,
-7.50949616528049));
#29100=CARTESIAN_POINT('Ctrl Pts',(-194.0750538067,-82.0173998381265,-7.68915683905057));
#29101=CARTESIAN_POINT('Ctrl Pts',(-194.665749224521,-81.13529176868,-7.85777298322919));
#29102=CARTESIAN_POINT('Ctrl Pts',(-195.248389252336,-80.2445949893091,
-8.00999044481605));
#29103=CARTESIAN_POINT('Ctrl Pts',(-195.822480593053,-79.3457729420087,
-8.14975356709067));
#29104=CARTESIAN_POINT('Ctrl Pts',(-196.650355260343,-78.0496168243568,
-8.35130049899169));
#29105=CARTESIAN_POINT('Ctrl Pts',(-197.460511393583,-76.7364778580625,
-8.52633259433118));
#29106=CARTESIAN_POINT('Ctrl Pts',(-198.252078897448,-75.4069267272506,
-8.68064281764092));
#29107=CARTESIAN_POINT('Ctrl Pts',(-198.594293956822,-74.8321274625641,
-8.74735510935841));
#29108=CARTESIAN_POINT('Ctrl Pts',(-198.933034987134,-74.2542612642923,
-8.81019436709263));
#29109=CARTESIAN_POINT('Ctrl Pts',(-199.268233060988,-73.6733769315866,
-8.86962868621838));
#29110=CARTESIAN_POINT('Ctrl Pts',(-199.712997529187,-72.9026185905557,
-8.94849033668896));
#29111=CARTESIAN_POINT('Ctrl Pts',(-200.151407978414,-72.1267399572591,
-9.02126337332997));
#29112=CARTESIAN_POINT('Ctrl Pts',(-200.583013021259,-71.3464384503323,
-9.08858769280887));
#29113=CARTESIAN_POINT('Ctrl Pts',(-201.014366027992,-70.5665926010997,
-9.15587269819712));
#29114=CARTESIAN_POINT('Ctrl Pts',(-201.438921493303,-69.7823291719526,
-9.21771534813081));
#29115=CARTESIAN_POINT('Ctrl Pts',(-201.85627383329,-68.9943705560089,-9.27475441892738));
#29116=CARTESIAN_POINT('Ctrl Pts',(-202.064023488162,-68.6021405028104,
-9.30314732855517));
#29117=CARTESIAN_POINT('Ctrl Pts',(-202.269989024108,-68.208995232856,-9.33034998358936));
#29118=CARTESIAN_POINT('Ctrl Pts',(-202.474124665087,-67.8150261129094,
-9.35644117223032));
#29119=CARTESIAN_POINT('Ctrl Pts',(-203.170724791756,-66.470631094265,-9.44547572408601));
#29120=CARTESIAN_POINT('Ctrl Pts',(-203.846736462659,-65.1152688211963,
-9.52164011411435));
#29121=CARTESIAN_POINT('Ctrl Pts',(-204.502059883097,-63.7490221183761,
-9.58726396269712));
#29122=CARTESIAN_POINT('Ctrl Pts',(-204.810586094828,-63.1057932845452,
-9.61815966514109));
#29123=CARTESIAN_POINT('Ctrl Pts',(-205.114526015695,-62.4601515926185,
-9.64671902957372));
#29124=CARTESIAN_POINT('Ctrl Pts',(-205.413865495665,-61.8121042464487,
-9.6731851612178));
#29125=CARTESIAN_POINT('Ctrl Pts',(-205.754227781708,-61.0752456261693,
-9.70327832858073));
#29126=CARTESIAN_POINT('Ctrl Pts',(-206.088782566592,-60.3349621177671,
-9.73065648355805));
#29127=CARTESIAN_POINT('Ctrl Pts',(-206.417157585293,-59.5920421271443,
-9.75556921716682));
#29128=CARTESIAN_POINT('Ctrl Pts',(-206.745708789431,-58.8487235322537,
-9.7804953173858));
#29129=CARTESIAN_POINT('Ctrl Pts',(-207.068073534945,-58.1027657529877,
-9.80295334994558));
#29130=CARTESIAN_POINT('Ctrl Pts',(-207.383926780309,-57.3549794466614,
-9.82319330782345));
#29131=CARTESIAN_POINT('Ctrl Pts',(-207.619735262604,-56.7967000667156,
-9.83830397652464));
#29132=CARTESIAN_POINT('Ctrl Pts',(-207.851915374644,-56.2374019541152,
-9.85217834393231));
#29133=CARTESIAN_POINT('Ctrl Pts',(-208.080349477207,-55.6774293990949,
-9.86492043799816));
#29134=CARTESIAN_POINT('Ctrl Pts',(-208.61075784454,-54.3772114135693,-9.89450670919867));
#29135=CARTESIAN_POINT('Ctrl Pts',(-209.121493376765,-53.0721049929371,
-9.91813719639479));
#29136=CARTESIAN_POINT('Ctrl Pts',(-209.61276822689,-51.7621815490425,-9.93682266532636));
#29137=CARTESIAN_POINT('Ctrl Pts',(-210.105670524664,-50.4479187178803,
-9.95557003366615));
#29138=CARTESIAN_POINT('Ctrl Pts',(-210.578983118157,-49.1288066369609,
-9.96933956672149));
#29139=CARTESIAN_POINT('Ctrl Pts',(-211.032876285271,-47.8048887258006,
-9.9791521086454));
#29140=CARTESIAN_POINT('Ctrl Pts',(-211.488405566466,-46.4761985887213,
-9.98900002109079));
#29141=CARTESIAN_POINT('Ctrl Pts',(-211.924375291595,-45.1426676490755,
-9.99486236406205));
#29142=CARTESIAN_POINT('Ctrl Pts',(-212.340911477666,-43.8043148655557,
-9.99777106082963));
#29143=CARTESIAN_POINT('Ctrl Pts',(-212.406256152434,-43.5943589714763,
-9.99822736654959));
#29144=CARTESIAN_POINT('Ctrl Pts',(-212.471122470112,-43.3842843658794,
-9.99861098248156));
#29145=CARTESIAN_POINT('Ctrl Pts',(-212.535510811764,-43.1740910731707,
-9.99892589262986));
#29146=CARTESIAN_POINT('Ctrl Pts',(-212.953022228768,-41.8111409298332,
-10.0009678551789));
#29147=CARTESIAN_POINT('Ctrl Pts',(-213.350438023984,-40.4432108877624,
-10.0000719408692));
#29148=CARTESIAN_POINT('Ctrl Pts',(-213.727826864813,-39.0703218294651,
-9.99695058699469));
#29149=CARTESIAN_POINT('Ctrl Pts',(-214.122785598877,-37.6335158993145,
-9.99368391389394));
#29150=CARTESIAN_POINT('Ctrl Pts',(-214.495809725065,-36.1912782559092,
-9.98797976034421));
#29151=CARTESIAN_POINT('Ctrl Pts',(-214.84691994715,-34.7436137410651,-9.98065477386882));
#29152=CARTESIAN_POINT('Ctrl Pts',(-215.198030169234,-33.295949226221,-9.97332978739343));
#29153=CARTESIAN_POINT('Ctrl Pts',(-215.527226576327,-31.8428574725277,
-9.96438396799237));
#29154=CARTESIAN_POINT('Ctrl Pts',(-215.834469144665,-30.3843292117711,
-9.95463396318898));
#29155=CARTESIAN_POINT('Ctrl Pts',(-216.12479711533,-29.006097177089,-9.94542072452923));
#29156=CARTESIAN_POINT('Ctrl Pts',(-216.395519847526,-27.6230191217557,
-9.93547880367801));
#29157=CARTESIAN_POINT('Ctrl Pts',(-216.646556008205,-26.235063563848,-9.9252656029735));
#29158=CARTESIAN_POINT('Ctrl Pts',(-216.897054662457,-24.8500798289305,
-9.91507427027801));
#29159=CARTESIAN_POINT('Ctrl Pts',(-217.127950993222,-23.4602391649776,
-9.904612818188));
#29160=CARTESIAN_POINT('Ctrl Pts',(-217.339112418497,-22.0655073883797,
-9.89433571722511));
#29161=CARTESIAN_POINT('Ctrl Pts',(-217.549435266681,-20.6763144554178,
-9.88409942931046));
#29162=CARTESIAN_POINT('Ctrl Pts',(-217.740179653031,-19.2822688917432,
-9.8740460312175));
#29163=CARTESIAN_POINT('Ctrl Pts',(-217.911162846412,-17.8833383662589,
-9.86462460047875));
#29164=CARTESIAN_POINT('Ctrl Pts',(-217.93455057477,-17.6919873540601,-9.86333590152238));
#29165=CARTESIAN_POINT('Ctrl Pts',(-217.957568495531,-17.500544951324,-9.86205902655124));
#29166=CARTESIAN_POINT('Ctrl Pts',(-217.980216065289,-17.3090110820993,
-9.86079512484355));
#29167=CARTESIAN_POINT('Ctrl Pts',(-218.144483248337,-15.9197790588204,
-9.85162780245975));
#29168=CARTESIAN_POINT('Ctrl Pts',(-218.289319103681,-14.5252556083932,
-9.84310086102437));
#29169=CARTESIAN_POINT('Ctrl Pts',(-218.414393171551,-13.1262875356464,
-9.83550018779937));
#29170=CARTESIAN_POINT('Ctrl Pts',(-218.487680928573,-12.3065554045771,
-9.831046536439));
#29171=CARTESIAN_POINT('Ctrl Pts',(-218.55418451901,-11.4852976098094,-9.82691091286767));
#29172=CARTESIAN_POINT('Ctrl Pts',(-218.613845276764,-10.6626873629055,
-9.82315083289945));
#29173=CARTESIAN_POINT('Ctrl Pts',(-218.714243156394,-9.2783884089601,-9.81682332265223));
#29174=CARTESIAN_POINT('Ctrl Pts',(-218.794867940585,-7.89578614496809,
-9.8115860039582));
#29175=CARTESIAN_POINT('Ctrl Pts',(-218.855960361108,-6.51486629004492,
-9.80756307330259));
#29176=CARTESIAN_POINT('Ctrl Pts',(-218.893128271323,-5.67473088955579,
-9.8051155696003));
#29177=CARTESIAN_POINT('Ctrl Pts',(-218.923065578444,-4.83521786741106,
-9.80311755493369));
#29178=CARTESIAN_POINT('Ctrl Pts',(-218.945817455584,-3.99632132774656,
-9.80159699667983));
#29179=CARTESIAN_POINT('Ctrl Pts',(-218.984176164557,-2.58197700676585,
-9.79903339934764));
#29180=CARTESIAN_POINT('Ctrl Pts',(-219.002113407906,-1.16938036292585,
-9.79787591200204));
#29181=CARTESIAN_POINT('Ctrl Pts',(-218.999802216758,0.241471131014165,
-9.79806426229321));
#29182=CARTESIAN_POINT('Ctrl Pts',(-218.997485328933,1.65580012391016,-9.79825307683448));
#29183=CARTESIAN_POINT('Ctrl Pts',(-218.974820086377,3.06837564753467,-9.7997943716916));
#29184=CARTESIAN_POINT('Ctrl Pts',(-218.931929074689,4.47920870148126,-9.80262742773335));
#29185=CARTESIAN_POINT('Ctrl Pts',(-218.888937672361,5.89334394924374,-9.80546711482199));
#29186=CARTESIAN_POINT('Ctrl Pts',(-218.825625720191,7.30572885744436,-9.80960461716078));
#29187=CARTESIAN_POINT('Ctrl Pts',(-218.742064526062,8.71637854307249,-9.81497878826245));
#29188=CARTESIAN_POINT('Ctrl Pts',(-218.731349327016,8.89726863592627,-9.81566792768488));
#29189=CARTESIAN_POINT('Ctrl Pts',(-218.720301091681,9.07813019772746,-9.81637740212719));
#29190=CARTESIAN_POINT('Ctrl Pts',(-218.708919908478,9.25896326123478,-9.81710708265811));
#29191=CARTESIAN_POINT('Ctrl Pts',(-218.619563682027,10.6787242724598,-9.8228359684512));
#29192=CARTESIAN_POINT('Ctrl Pts',(-218.509688811122,12.0967197729986,-9.8298080272327));
#29193=CARTESIAN_POINT('Ctrl Pts',(-218.379310061933,13.5129542311266,-9.83770685533299));
#29194=CARTESIAN_POINT('Ctrl Pts',(-218.242405787213,15.0000719748565,-9.84600102396813));
#29195=CARTESIAN_POINT('Ctrl Pts',(-218.0828942667,16.4852483906094,-9.8553170541224));
#29196=CARTESIAN_POINT('Ctrl Pts',(-217.900731068501,17.9684821506137,-9.86528861611505));
#29197=CARTESIAN_POINT('Ctrl Pts',(-217.718567870302,19.451715910618,-9.8752601781077));
#29198=CARTESIAN_POINT('Ctrl Pts',(-217.513752947392,20.9330073981508,-9.88588727193872));
#29199=CARTESIAN_POINT('Ctrl Pts',(-217.286179447546,22.4123429600545,-9.89680356792739));
#29200=CARTESIAN_POINT('Ctrl Pts',(-217.074537568303,23.7881154404372,-9.90695565241428));
#29201=CARTESIAN_POINT('Ctrl Pts',(-216.843213111179,25.1621874059895,-9.91736416322261));
#29202=CARTESIAN_POINT('Ctrl Pts',(-216.592066415917,26.5345652905463,-9.92749162982048));
#29203=CARTESIAN_POINT('Ctrl Pts',(-216.341668290249,27.9028526559885,-9.93758891042062));
#29204=CARTESIAN_POINT('Ctrl Pts',(-216.071565840309,29.2694562987497,-9.94740681967818));
#29205=CARTESIAN_POINT('Ctrl Pts',(-215.781572186617,30.6343644735032,-9.95641267871605));
#29206=CARTESIAN_POINT('Ctrl Pts',(-215.493060155512,31.9922991205487,-9.96537252542233));
#29207=CARTESIAN_POINT('Ctrl Pts',(-215.184859557881,33.3485558414738,-9.97352859849281));
#29208=CARTESIAN_POINT('Ctrl Pts',(-214.856739636078,34.703101119423,-9.98035634202435));
#29209=CARTESIAN_POINT('Ctrl Pts',(-214.795334533757,34.9565937782491,-9.9816341013505));
#29210=CARTESIAN_POINT('Ctrl Pts',(-214.733231682609,35.2100264299969,-9.98286533962214));
#29211=CARTESIAN_POINT('Ctrl Pts',(-214.670429391573,35.4633987574771,-9.98404661882751));
#29212=CARTESIAN_POINT('Ctrl Pts',(-214.359497476236,36.7178361637757,-9.98989509027358));
#29213=CARTESIAN_POINT('Ctrl Pts',(-214.032421066029,37.9667411686325,-9.99445006270918));
#29214=CARTESIAN_POINT('Ctrl Pts',(-213.689538210722,39.2093446217989,-9.99716936427343));
#29215=CARTESIAN_POINT('Ctrl Pts',(-213.440231444473,40.1128294238039,-9.99914654181073));
#29216=CARTESIAN_POINT('Ctrl Pts',(-213.182569462386,41.0129832213348,-10.0001532732747));
#29217=CARTESIAN_POINT('Ctrl Pts',(-212.916698050239,41.9095173135889,-9.99998115667634));
#29218=CARTESIAN_POINT('Ctrl Pts',(-212.509602595805,43.2822672108238,-9.99971761617662));
#29219=CARTESIAN_POINT('Ctrl Pts',(-212.083102729471,44.647086672049,-9.99669713415972));
#29220=CARTESIAN_POINT('Ctrl Pts',(-211.63735202868,46.004008185371,-9.99003728668321));
#29221=CARTESIAN_POINT('Ctrl Pts',(-211.391599599651,46.752109662965,-9.98636556235074));
#29222=CARTESIAN_POINT('Ctrl Pts',(-211.139994833097,47.4978104022167,-9.98158762888982));
#29223=CARTESIAN_POINT('Ctrl Pts',(-210.882556783091,48.2411147726525,-9.9755556113417));
#29224=CARTESIAN_POINT('Ctrl Pts',(-210.407166434106,49.6137157694966,-9.96441676482224));
#29225=CARTESIAN_POINT('Ctrl Pts',(-209.911886250968,50.9781493632379,-9.9491269391516));
#29226=CARTESIAN_POINT('Ctrl Pts',(-209.396804182012,52.3344093849598,-9.92839606297258));
#29227=CARTESIAN_POINT('Ctrl Pts',(-208.869479898179,53.7229043214992,-9.90717246562135));
#29228=CARTESIAN_POINT('Ctrl Pts',(-208.321401349102,55.1028329191272,-9.88024610376969));
#29229=CARTESIAN_POINT('Ctrl Pts',(-207.752608950314,56.4741717378989,-9.84623271715167));
#29230=CARTESIAN_POINT('Ctrl Pts',(-207.183816551525,57.8455105566706,-9.81221933053365));
#29231=CARTESIAN_POINT('Ctrl Pts',(-206.594310169254,59.2082599190967,-9.77111891914926));
#29232=CARTESIAN_POINT('Ctrl Pts',(-205.984077548804,60.5623745285646,-9.72154722273255));
#29233=CARTESIAN_POINT('Ctrl Pts',(-205.383262636071,61.8955911145903,-9.6727405653063));
#29234=CARTESIAN_POINT('Ctrl Pts',(-204.76235657447,63.2204360342108,-9.61598017611668));
#29235=CARTESIAN_POINT('Ctrl Pts',(-204.121307325464,64.536826706914,-9.54877517923461));
#29236=CARTESIAN_POINT('Ctrl Pts',(-203.472743362976,65.8686487973313,-9.48078237034439));
#29237=CARTESIAN_POINT('Ctrl Pts',(-202.803561129253,67.1918176216725,-9.40209864421725));
#29238=CARTESIAN_POINT('Ctrl Pts',(-202.11366114301,68.5062179193968,-9.31014449600325));
#29239=CARTESIAN_POINT('Ctrl Pts',(-201.423761156767,69.8206182171212,-9.21819034778924));
#29240=CARTESIAN_POINT('Ctrl Pts',(-200.713143257863,71.1262502867284,-9.11296577748836));
#29241=CARTESIAN_POINT('Ctrl Pts',(-199.981664414448,72.4229644761836,-8.99189128025066));
#29242=CARTESIAN_POINT('Ctrl Pts',(-199.6776144015,72.961962930674,-8.94156487261202));
#29243=CARTESIAN_POINT('Ctrl Pts',(-199.369834898682,73.4996320589593,-8.88837986748052));
#29244=CARTESIAN_POINT('Ctrl Pts',(-199.058853023589,74.0350386097636,-8.83213170660312));
#29245=CARTESIAN_POINT('Ctrl Pts',(-198.810885502973,74.4619555639597,-8.78728112813178));
#29246=CARTESIAN_POINT('Ctrl Pts',(-198.560882815212,74.8874344426336,-8.74048300008057));
#29247=CARTESIAN_POINT('Ctrl Pts',(-198.30913267803,75.3110141404511,-8.69163361829107));
#29248=CARTESIAN_POINT('Ctrl Pts',(-197.74165679773,76.2658150576885,-8.58152108272949));
#29249=CARTESIAN_POINT('Ctrl Pts',(-197.164705398621,77.2119850731197,-8.46091798763827));
#29250=CARTESIAN_POINT('Ctrl Pts',(-196.578625312678,78.1492963793824,-8.32767843937961));
#29251=CARTESIAN_POINT('Ctrl Pts',(-195.949038803721,79.1561870198767,-8.18454813337673));
#29252=CARTESIAN_POINT('Ctrl Pts',(-195.308874570202,80.1529188927709,-8.02725639835802));
#29253=CARTESIAN_POINT('Ctrl Pts',(-194.658762385835,81.1389439920761,-7.85130852010962));
#29254=CARTESIAN_POINT('Ctrl Pts',(-194.098499825935,81.9886941729618,-7.69967775384069));
#29255=CARTESIAN_POINT('Ctrl Pts',(-193.530849705582,82.8304930966393,-7.53419128798475));
#29256=CARTESIAN_POINT('Ctrl Pts',(-192.956236453638,83.6640125707261,-7.35197230730516));
#29257=CARTESIAN_POINT('Ctrl Pts',(-192.419403832868,84.442728415206,-7.18173416430839));
#29258=CARTESIAN_POINT('Ctrl Pts',(-191.876510663817,85.2141889951778,-6.99671260528906));
#29259=CARTESIAN_POINT('Ctrl Pts',(-191.328162094401,85.977819963292,-6.79234392467887));
#29260=CARTESIAN_POINT('Ctrl Pts',(-191.242507083244,86.0971032490376,-6.76042043186023));
#29261=CARTESIAN_POINT('Ctrl Pts',(-191.156719036077,86.2161955608546,-6.72802486677896));
#29262=CARTESIAN_POINT('Ctrl Pts',(-191.070800343556,86.3350947874365,-6.69513983518131));
#29263=CARTESIAN_POINT('Ctrl Pts',(-190.608513931787,86.9748333030743,-6.51820158330396));
#29264=CARTESIAN_POINT('Ctrl Pts',(-190.142422121888,87.609006867386,-6.32728225133389));
#29265=CARTESIAN_POINT('Ctrl Pts',(-189.673163685796,88.2369638600037,-6.11735698536059));
#29266=CARTESIAN_POINT('Ctrl Pts',(-189.496875586272,88.4728708491959,-6.03849356313051));
#29267=CARTESIAN_POINT('Ctrl Pts',(-189.320140977775,88.707900834228,-5.95694781816414));
#29268=CARTESIAN_POINT('Ctrl Pts',(-189.142995147248,88.9420205250928,-5.87245333700276));
#29269=CARTESIAN_POINT('Ctrl Pts',(-188.818651423809,89.3706800766031,-5.717748851165));
#29270=CARTESIAN_POINT('Ctrl Pts',(-188.49293989293,89.7962712759086,-5.55305032555424));
#29271=CARTESIAN_POINT('Ctrl Pts',(-188.166231145434,90.2184105278924,-5.37541261640281));
#29272=CARTESIAN_POINT('Ctrl Pts',(-187.941553999842,90.5087150970382,-5.25325141396333));
#29273=CARTESIAN_POINT('Ctrl Pts',(-187.716679186465,90.7970273844016,-5.12511114867476));
#29274=CARTESIAN_POINT('Ctrl Pts',(-187.492754926394,91.0819602571486,-4.99016685446453));
#29275=CARTESIAN_POINT('Ctrl Pts',(-187.391065228939,91.2113555161321,-4.92888522090169));
#29276=CARTESIAN_POINT('Ctrl Pts',(-187.289572125172,91.3400542891487,-4.86620039318761));
#29277=CARTESIAN_POINT('Ctrl Pts',(-187.188385892342,91.467928897974,-4.80203510975558));
#29278=CARTESIAN_POINT('Ctrl Pts',(-186.926482284857,91.798910894441,-4.63595402603387));
#29279=CARTESIAN_POINT('Ctrl Pts',(-186.666166588022,92.1249576589846,-4.45982540733765));
#29280=CARTESIAN_POINT('Ctrl Pts',(-186.408598112086,92.4448486891005,-4.27016769975641));
#29281=CARTESIAN_POINT('Ctrl Pts',(-186.347527747809,92.520695943571,-4.22519921031799));
#29282=CARTESIAN_POINT('Ctrl Pts',(-186.286612000581,92.5961972877401,-4.17947014218683));
#29283=CARTESIAN_POINT('Ctrl Pts',(-186.225866640945,92.6713367351173,-4.13293408803839));
#29284=CARTESIAN_POINT('Ctrl Pts',(-186.010419293658,92.9378360152417,-3.96788330095816));
#29285=CARTESIAN_POINT('Ctrl Pts',(-185.797040930281,93.1998680077896,-3.79291563167685));
#29286=CARTESIAN_POINT('Ctrl Pts',(-185.587151181677,93.4558788066831,-3.60367209755208));
#29287=CARTESIAN_POINT('Ctrl Pts',(-185.488273569283,93.576483727648,-3.5145207743467));
#29288=CARTESIAN_POINT('Ctrl Pts',(-185.390170766711,93.6957528796746,-3.4222012268844));
#29289=CARTESIAN_POINT('Ctrl Pts',(-185.292994175947,93.8135264201691,-3.32625772752428));
#29290=CARTESIAN_POINT('Ctrl Pts',(-185.162032493132,93.9722459320697,-3.19695784128052));
#29291=CARTESIAN_POINT('Ctrl Pts',(-185.032274848444,94.1288222169724,-3.0606810953648));
#29292=CARTESIAN_POINT('Ctrl Pts',(-184.905880009225,94.2807288539447,-2.91629164267507));
#29293=CARTESIAN_POINT('Ctrl Pts',(-184.773357322611,94.4400001957996,-2.7649019316134));
#29294=CARTESIAN_POINT('Ctrl Pts',(-184.644531572858,94.5941382067379,-2.60459380798681));
#29295=CARTESIAN_POINT('Ctrl Pts',(-184.52193501311,94.7402683921781,-2.43405808220338));
#29296=CARTESIAN_POINT('Ctrl Pts',(-184.490522330022,94.777711051371,-2.39036203787495));
#29297=CARTESIAN_POINT('Ctrl Pts',(-184.459518816605,94.8146281515711,-2.34599452244704));
#29298=CARTESIAN_POINT('Ctrl Pts',(-184.42896747061,94.8509716846399,-2.30093351259949));
#29299=CARTESIAN_POINT('Ctrl Pts',(-184.312740025998,94.9892345283602,-2.12950649831777));
#29300=CARTESIAN_POINT('Ctrl Pts',(-184.202585838296,95.1197493985745,-1.94735170602647));
#29301=CARTESIAN_POINT('Ctrl Pts',(-184.102034801778,95.2385318422614,-1.74979548300606));
#29302=CARTESIAN_POINT('Ctrl Pts',(-184.088602492028,95.2543996307167,-1.72340454291751));
#29303=CARTESIAN_POINT('Ctrl Pts',(-184.075341611869,95.2700580979542,-1.6967387568678));
#29304=CARTESIAN_POINT('Ctrl Pts',(-184.062260624235,95.2854977874351,-1.66978698322322));
#29305=CARTESIAN_POINT('Ctrl Pts',(-183.951258512844,95.4165152747594,-1.44108072159684));
#29306=CARTESIAN_POINT('Ctrl Pts',(-183.856402416991,95.5280069404102,-1.19842060958046));
#29307=CARTESIAN_POINT('Ctrl Pts',(-183.78559008165,95.6110982791194,-0.935265073867139));
#29308=CARTESIAN_POINT('Ctrl Pts',(-183.75018391398,95.6526439484739,-0.803687306010473));
#29309=CARTESIAN_POINT('Ctrl Pts',(-183.720972654883,95.6868740766621,-0.666464316175631));
#29310=CARTESIAN_POINT('Ctrl Pts',(-183.700029885832,95.711403889144,-0.528231852282087));
#29311=CARTESIAN_POINT('Ctrl Pts',(-183.67908711678,95.7359337016259,-0.389999388388542));
#29312=CARTESIAN_POINT('Ctrl Pts',(-183.666054681306,95.7511842509038,-0.249647095948257));
#29313=CARTESIAN_POINT('Ctrl Pts',(-183.66168335083,95.7563001446319,-0.106977127421175));
#29314=CARTESIAN_POINT('Ctrl Pts',(-183.657312020355,95.7614160383599,0.0356928411059037));
#29315=CARTESIAN_POINT('Ctrl Pts',(-183.661865337804,95.7560891876555,0.179679148990217));
#29316=CARTESIAN_POINT('Ctrl Pts',(-183.674665679525,95.7411044663663,0.319496061024171));
#29317=CARTESIAN_POINT('Ctrl Pts',(-183.687466021247,95.7261197450771,0.459312973058134));
#29318=CARTESIAN_POINT('Ctrl Pts',(-183.708428755956,95.7015755681125,0.596571383448631));
#29319=CARTESIAN_POINT('Ctrl Pts',(-183.73677770673,95.6683452210586,0.731509051287532));
#29320=CARTESIAN_POINT('Ctrl Pts',(-183.765126657504,95.6351148740048,0.866446719126424));
#29321=CARTESIAN_POINT('Ctrl Pts',(-183.801164672152,95.5928412644945,0.999673886209484));
#29322=CARTESIAN_POINT('Ctrl Pts',(-183.842486096339,95.544296113797,1.12685895415084));
#29323=CARTESIAN_POINT('Ctrl Pts',(-183.883807520525,95.4957509630995,1.25404402209221));
#29324=CARTESIAN_POINT('Ctrl Pts',(-183.930563125213,95.4407576673987,1.37625930381363));
#29325=CARTESIAN_POINT('Ctrl Pts',(-183.981732092056,95.3804654898362,1.49441051952705));
#29326=CARTESIAN_POINT('Ctrl Pts',(-184.05777694133,95.2908621650469,1.67000115472771));
#29327=CARTESIAN_POINT('Ctrl Pts',(-184.143477886773,95.189658168371,1.83625903517367));
#29328=CARTESIAN_POINT('Ctrl Pts',(-184.234795490352,95.0814776257665,1.99288757663377));
#29329=CARTESIAN_POINT('Ctrl Pts',(-184.266369245604,95.044073381225,2.04704308487863));
#29330=CARTESIAN_POINT('Ctrl Pts',(-184.298614785763,95.0058353815126,2.10004742185922));
#29331=CARTESIAN_POINT('Ctrl Pts',(-184.331366318257,94.9669557749258,2.15188832834384));
#29332=CARTESIAN_POINT('Ctrl Pts',(-184.458841821245,94.8156285841579,2.35366348591041));
#29333=CARTESIAN_POINT('Ctrl Pts',(-184.595169875239,94.653167207116,2.54014556267795));
#29334=CARTESIAN_POINT('Ctrl Pts',(-184.737488050318,94.4827425911459,2.71592585637909));
#29335=CARTESIAN_POINT('Ctrl Pts',(-184.85791892067,94.3385278074816,2.86467266084904));
#29336=CARTESIAN_POINT('Ctrl Pts',(-184.982907743565,94.1882878961831,3.00586283997828));
#29337=CARTESIAN_POINT('Ctrl Pts',(-185.110153711901,94.0346817681954,3.13988186032778));
#29338=CARTESIAN_POINT('Ctrl Pts',(-185.133279603762,94.0067651375047,3.16423869781617));
#29339=CARTESIAN_POINT('Ctrl Pts',(-185.156480155079,93.9787374103966,3.18835867174178));
#29340=CARTESIAN_POINT('Ctrl Pts',(-185.179741698894,93.9506146703416,3.21224409603392));
#29341=CARTESIAN_POINT('Ctrl Pts',(-185.375067641756,93.714469521897,3.4128087299952));
#29342=CARTESIAN_POINT('Ctrl Pts',(-185.57531853868,93.470864259905,3.59807650580166));
#29343=CARTESIAN_POINT('Ctrl Pts',(-185.778946495124,93.2214476654712,3.7719301043373));
#29344=CARTESIAN_POINT('Ctrl Pts',(-185.890683969115,93.0845844335245,3.86732939176304));
#29345=CARTESIAN_POINT('Ctrl Pts',(-186.003438949569,92.9459719373273,3.95929177436257));
#29346=CARTESIAN_POINT('Ctrl Pts',(-186.116960759486,92.8058870467681,4.04845878075692));
#29347=CARTESIAN_POINT('Ctrl Pts',(-186.336052281991,92.5355300821047,4.2205467275774));
#29348=CARTESIAN_POINT('Ctrl Pts',(-186.556974212558,92.2609504033717,4.38110940427998));
#29349=CARTESIAN_POINT('Ctrl Pts',(-186.778501492463,91.9835506512719,4.53240916560392));
#29350=CARTESIAN_POINT('Ctrl Pts',(-186.880937788642,91.8552783988506,4.60237159718119));
#29351=CARTESIAN_POINT('Ctrl Pts',(-186.983504074352,91.7264036161273,4.67035340948399));
#29352=CARTESIAN_POINT('Ctrl Pts',(-187.086082139975,91.5970674043341,4.73657828946882));
#29353=CARTESIAN_POINT('Ctrl Pts',(-187.410494074091,91.1880305370078,4.94602015476302));
#29354=CARTESIAN_POINT('Ctrl Pts',(-187.735717460477,90.7735000599875,5.13817049334406));
#29355=CARTESIAN_POINT('Ctrl Pts',(-188.06083509298,90.3544283086145,5.31766757924143));
#29356=CARTESIAN_POINT('Ctrl Pts',(-188.145233520197,90.2455348162912,5.3635191399407));
#29357=CARTESIAN_POINT('Ctrl Pts',(-187.854664851553,90.6205738707536,6.83263373170868));
#29358=CARTESIAN_POINT('Ctrl Pts',(-188.302848962895,91.4632161367811,8.04608569871648));
#29359=CARTESIAN_POINT('Ctrl Pts',(-187.791407151483,90.7024945656512,5.17051448656997));
#29360=CARTESIAN_POINT('Ctrl Pts',(-187.496540276221,91.0800720173262,6.57808105135662));
#29361=CARTESIAN_POINT('Ctrl Pts',(-187.88687547988,91.8985142221956,7.75653201531377));
#29362=CARTESIAN_POINT('Ctrl Pts',(-187.437220699584,91.1543549984681,4.9629292066438));
#29363=CARTESIAN_POINT('Ctrl Pts',(-187.136870690502,91.5359208617972,6.30546516147755));
#29364=CARTESIAN_POINT('Ctrl Pts',(-187.47070368759,92.3280722645737,7.44513708416162));
#29365=CARTESIAN_POINT('Ctrl Pts',(-186.758422149138,92.0101784299077,4.52454213939994));
#29366=CARTESIAN_POINT('Ctrl Pts',(-186.447354126494,92.3993958986497,5.73365867686477));
#29367=CARTESIAN_POINT('Ctrl Pts',(-186.673417663121,93.1401290348249,6.78749067092915));
#29368=CARTESIAN_POINT('Ctrl Pts',(-186.432985631702,92.4159647578489,4.29662116512001));
#29369=CARTESIAN_POINT('Ctrl Pts',(-186.116813727194,92.8087490972247,5.43831752668723));
#29370=CARTESIAN_POINT('Ctrl Pts',(-186.291328581577,93.5244589650537,6.44557505453847));
#29371=CARTESIAN_POINT('Ctrl Pts',(-185.789504878419,93.2099142476764,3.79054251520617));
#29372=CARTESIAN_POINT('Ctrl Pts',(-185.463263222825,93.6095176182921,4.78647394195717));
#29373=CARTESIAN_POINT('Ctrl Pts',(-185.53612909977,94.2750879221146,5.68638123862275));
#29374=CARTESIAN_POINT('Ctrl Pts',(-185.473492555278,93.5955608302612,3.5147156518481));
#29375=CARTESIAN_POINT('Ctrl Pts',(-185.142185731736,93.9986018940583,4.43322287886808));
#29376=CARTESIAN_POINT('Ctrl Pts',(-185.165403861164,94.6390060126994,5.27259965429573));
#29377=CARTESIAN_POINT('Ctrl Pts',(-185.016589769184,94.1478172607574,3.04374369325038));
#29378=CARTESIAN_POINT('Ctrl Pts',(-184.677473990833,94.5562789886833,3.83252013850768));
#29379=CARTESIAN_POINT('Ctrl Pts',(-184.629593327285,95.1592700205275,4.56607106412171));
#29380=CARTESIAN_POINT('Ctrl Pts',(-184.866799006187,94.3279436322682,2.87648998617678));
#29381=CARTESIAN_POINT('Ctrl Pts',(-184.52529718626,94.7379585618407,3.6200170612726));
#29382=CARTESIAN_POINT('Ctrl Pts',(-184.453967955319,95.3288078676141,4.31516546799618));
#29383=CARTESIAN_POINT('Ctrl Pts',(-184.579916698489,94.6713779749968,2.5196724298392));
#29384=CARTESIAN_POINT('Ctrl Pts',(-184.233884394348,95.0842876797572,3.16778187881883));
#29385=CARTESIAN_POINT('Ctrl Pts',(-184.117665437549,95.6517941247141,3.77988572544218));
#29386=CARTESIAN_POINT('Ctrl Pts',(-184.44239986753,94.8352001907092,2.32993307581778));
#29387=CARTESIAN_POINT('Ctrl Pts',(-184.094156916584,95.2495304257977,2.9278452901178));
#29388=CARTESIAN_POINT('Ctrl Pts',(-183.956489556471,95.8057270256804,3.49524829819147));
#29389=CARTESIAN_POINT('Ctrl Pts',(-184.185294918109,95.1402973045157,1.91734932039146));
#29390=CARTESIAN_POINT('Ctrl Pts',(-183.832981297565,95.5571842813552,2.40725694755477));
#29391=CARTESIAN_POINT('Ctrl Pts',(-183.655197053014,96.0922042485234,2.87631092236716));
#29392=CARTESIAN_POINT('Ctrl Pts',(-184.064453461112,95.2830402548575,1.69197261173593));
#29393=CARTESIAN_POINT('Ctrl Pts',(-183.710171068013,95.7011829603298,2.12341452229605));
#29394=CARTESIAN_POINT('Ctrl Pts',(-183.513612438245,96.2261237477396,2.53821212995774));
#29395=CARTESIAN_POINT('Ctrl Pts',(-183.911202264701,95.4635408941671,1.32666688325273));
#29396=CARTESIAN_POINT('Ctrl Pts',(-183.554420819748,95.8832673602713,1.66399482314503));
#29397=CARTESIAN_POINT('Ctrl Pts',(-183.334075436563,96.3953763623405,1.99019884061584));
#29398=CARTESIAN_POINT('Ctrl Pts',(-183.864744551489,95.5181608807362,1.20034832248043));
#29399=CARTESIAN_POINT('Ctrl Pts',(-183.507217373514,95.9383518302635,1.50531552343668));
#29400=CARTESIAN_POINT('Ctrl Pts',(-183.279653114889,96.4465756811072,1.80070209637048));
#29401=CARTESIAN_POINT('Ctrl Pts',(-183.783468331685,95.6136084402799,0.936341958789021));
#29402=CARTESIAN_POINT('Ctrl Pts',(-183.424650598207,96.0345934282162,1.17391428722675));
#29403=CARTESIAN_POINT('Ctrl Pts',(-183.184447352807,96.5360269050087,1.40465304838242));
#29404=CARTESIAN_POINT('Ctrl Pts',(-183.748737326012,95.654333157593,0.798204067099665));
#29405=CARTESIAN_POINT('Ctrl Pts',(-183.389359661152,96.075666167106,1.0006029019253));
#29406=CARTESIAN_POINT('Ctrl Pts',(-183.143766417956,96.5741824061768,1.1974255383652));
#29407=CARTESIAN_POINT('Ctrl Pts',(-183.695928409161,95.7162162993234,0.518880068927119));
#29408=CARTESIAN_POINT('Ctrl Pts',(-183.335711711721,96.1380633310152,0.650342007065702));
#29409=CARTESIAN_POINT('Ctrl Pts',(-183.081912119256,96.6321546625029,0.778397747287054));
#29410=CARTESIAN_POINT('Ctrl Pts',(-183.677440490251,95.7378571902513,0.376560792571389));
#29411=CARTESIAN_POINT('Ctrl Pts',(-183.316924770873,96.1598898803611,0.471927258717125));
#29412=CARTESIAN_POINT('Ctrl Pts',(-183.060258441793,96.6524237482766,0.564897533939989));
#29413=CARTESIAN_POINT('Ctrl Pts',(-183.658185995667,95.760394199856,0.0859862681696598));
#29414=CARTESIAN_POINT('Ctrl Pts',(-183.297364262565,96.1826139348272,0.107762579034491));
#29415=CARTESIAN_POINT('Ctrl Pts',(-183.037706970332,96.6735319375049,0.128992270488467));
#29416=CARTESIAN_POINT('Ctrl Pts',(-183.657681880049,95.7609839412904,-0.063896210583788));
#29417=CARTESIAN_POINT('Ctrl Pts',(-183.296852000031,96.1832087243297,-0.0800795353757084));
#29418=CARTESIAN_POINT('Ctrl Pts',(-183.037116546925,96.6740842350221,-0.0958538786891257));
#29419=CARTESIAN_POINT('Ctrl Pts',(-183.675244045363,95.7404283569817,-0.355921350698398));
#29420=CARTESIAN_POINT('Ctrl Pts',(-183.31469328487,96.162482543441,-0.44605714576703));
#29421=CARTESIAN_POINT('Ctrl Pts',(-183.057685885535,96.6548319532991,-0.533935282757487));
#29422=CARTESIAN_POINT('Ctrl Pts',(-183.693020864062,95.7196211416447,-0.499360341536995));
#29423=CARTESIAN_POINT('Ctrl Pts',(-183.33275775371,96.141496684891,-0.625871301849139));
#29424=CARTESIAN_POINT('Ctrl Pts',(-183.0785066467,96.6353439239973,-0.749115235509941));
#29425=CARTESIAN_POINT('Ctrl Pts',(-183.744901665609,95.6588299326157,-0.78155798871691));
#29426=CARTESIAN_POINT('Ctrl Pts',(-183.385462858047,96.0802005494342,-0.979723363419466));
#29427=CARTESIAN_POINT('Ctrl Pts',(-183.139273685515,96.5783953473938,-1.17245393006151));
#29428=CARTESIAN_POINT('Ctrl Pts',(-183.779175195977,95.618644870505,-0.920237396574461));
#29429=CARTESIAN_POINT('Ctrl Pts',(-183.420288799078,96.0396722809014,-1.15370660831193));
#29430=CARTESIAN_POINT('Ctrl Pts',(-183.179418644892,96.5407460179378,-1.38049379518866));
#29431=CARTESIAN_POINT('Ctrl Pts',(-183.85908515349,95.524811693759,-1.18387312000799));
#29432=CARTESIAN_POINT('Ctrl Pts',(-183.501467654743,95.9450585544367,-1.48462552841789));
#29433=CARTESIAN_POINT('Ctrl Pts',(-183.273023596524,96.4528094730268,-1.77598682731276));
#29434=CARTESIAN_POINT('Ctrl Pts',(-183.9049533987,95.4708918026245,-1.3102946528729));
#29435=CARTESIAN_POINT('Ctrl Pts',(-183.548072370971,95.8906799738278,-1.64342456925302));
#29436=CARTESIAN_POINT('Ctrl Pts',(-183.326755114843,96.4022676282472,-1.9656380451627));
#29437=CARTESIAN_POINT('Ctrl Pts',(-184.006197987058,95.3516620124118,-1.55440286313822));
#29438=CARTESIAN_POINT('Ctrl Pts',(-183.650923334156,95.7704563495827,-1.95026772005439));
#29439=CARTESIAN_POINT('Ctrl Pts',(-183.445364605803,96.2904706695442,-2.33183688685736));
#29440=CARTESIAN_POINT('Ctrl Pts',(-184.061902804819,95.2859635471583,-1.67265649549514));
#29441=CARTESIAN_POINT('Ctrl Pts',(-183.707519331346,95.7042005353516,-2.09904096749872));
#29442=CARTESIAN_POINT('Ctrl Pts',(-183.510627455621,96.2288509060907,-2.50923503171724));
#29443=CARTESIAN_POINT('Ctrl Pts',(-184.238169879718,95.07765401711,-2.01149467785066));
#29444=CARTESIAN_POINT('Ctrl Pts',(-183.886670042307,95.4940451899596,-2.52591331873638));
#29445=CARTESIAN_POINT('Ctrl Pts',(-183.717155446954,96.0334014306346,-3.017543046058));
#29446=CARTESIAN_POINT('Ctrl Pts',(-184.367342568346,94.9244689409693,-2.21657754164571));
#29447=CARTESIAN_POINT('Ctrl Pts',(-184.017930454936,95.3395258984641,-2.78467603615262));
#29448=CARTESIAN_POINT('Ctrl Pts',(-183.868524764247,95.8895820176952,-3.32519803265031));
#29449=CARTESIAN_POINT('Ctrl Pts',(-184.640230357973,94.5993241361901,-2.59999275069374));
#29450=CARTESIAN_POINT('Ctrl Pts',(-184.295133716673,95.0116489254231,-3.26945356760231));
#29451=CARTESIAN_POINT('Ctrl Pts',(-184.188363389419,95.5840555999993,-3.90037822873724));
#29452=CARTESIAN_POINT('Ctrl Pts',(-184.78434203569,94.426893415286,-2.77839839816462));
#29453=CARTESIAN_POINT('Ctrl Pts',(-184.441552692558,94.8377263261817,-3.49555218419125));
#29454=CARTESIAN_POINT('Ctrl Pts',(-184.357297442187,95.4219062735372,-4.1680134022079));
#29455=CARTESIAN_POINT('Ctrl Pts',(-185.081686343193,94.0693232210915,-3.1143754936061));
#29456=CARTESIAN_POINT('Ctrl Pts',(-184.743586343125,94.4771334873336,-3.92236858029529));
#29457=CARTESIAN_POINT('Ctrl Pts',(-184.705925080379,95.0853544967748,-4.67202934040196));
#29458=CARTESIAN_POINT('Ctrl Pts',(-185.233416268676,93.8859970214969,-3.27026141835536));
#29459=CARTESIAN_POINT('Ctrl Pts',(-184.897720023963,94.2922334135553,-4.12090822859617));
#29460=CARTESIAN_POINT('Ctrl Pts',(-184.883856541663,94.9126597774132,-4.90588156360651));
#29461=CARTESIAN_POINT('Ctrl Pts',(-185.69467972387,93.3258217356729,-3.71184482224262));
#29462=CARTESIAN_POINT('Ctrl Pts',(-185.366864517595,93.7265360394383,-4.6855524165187));
#29463=CARTESIAN_POINT('Ctrl Pts',(-185.424878850264,94.3844962534327,-5.56832292611329));
#29464=CARTESIAN_POINT('Ctrl Pts',(-186.010146579491,92.9389319284735,-3.97193425575934));
#29465=CARTESIAN_POINT('Ctrl Pts',(-185.687350973287,93.3362230628123,-5.01951580728777));
#29466=CARTESIAN_POINT('Ctrl Pts',(-185.795033412765,94.0190928215223,-5.95849601722182));
#29467=CARTESIAN_POINT('Ctrl Pts',(-186.648836664447,92.1470885487441,-4.45009979324727));
#29468=CARTESIAN_POINT('Ctrl Pts',(-186.336019695174,92.5375609708031,-5.63706525171897));
#29469=CARTESIAN_POINT('Ctrl Pts',(-186.544745323736,93.2698431415528,-6.67581600087155));
#29470=CARTESIAN_POINT('Ctrl Pts',(-186.972201554671,91.741974605203,-4.66770157630044));
#29471=CARTESIAN_POINT('Ctrl Pts',(-186.664462004782,92.1288597295902,-5.91981377516862));
#29472=CARTESIAN_POINT('Ctrl Pts',(-186.924468369905,92.8858476278282,-7.00225129807417));
#29473=CARTESIAN_POINT('Ctrl Pts',(-187.622975925479,90.9175328418992,-5.07270906192872));
#29474=CARTESIAN_POINT('Ctrl Pts',(-187.325327673611,91.2972402661008,-6.44944820677759));
#29475=CARTESIAN_POINT('Ctrl Pts',(-187.688972154269,92.1029529048828,-7.60982332854755));
#29476=CARTESIAN_POINT('Ctrl Pts',(-187.951135111485,90.4972347714145,-5.26033203020097));
#29477=CARTESIAN_POINT('Ctrl Pts',(-187.658573120978,90.8732133787086,-6.69644438830181));
#29478=CARTESIAN_POINT('Ctrl Pts',(-188.074634250876,91.7031292223758,-7.89128595957309));
#29479=CARTESIAN_POINT('Ctrl Pts',(-188.605044860185,89.6501506723977,-5.61022454744543));
#29480=CARTESIAN_POINT('Ctrl Pts',(-188.322538615507,90.0186811388234,-7.16027924921534));
#29481=CARTESIAN_POINT('Ctrl Pts',(-188.843435098385,90.8958628411168,-8.41617737112857));
#29482=CARTESIAN_POINT('Ctrl Pts',(-188.930864921547,89.2233084878171,-5.77255548082708));
#29483=CARTESIAN_POINT('Ctrl Pts',(-188.653339852176,89.5880484625308,-7.37702489960499));
#29484=CARTESIAN_POINT('Ctrl Pts',(-189.226654411641,90.4883717460544,-8.65969820825197));
#29485=CARTESIAN_POINT('Ctrl Pts',(-189.903920178562,87.9339173140976,-6.23019362937991));
#29486=CARTESIAN_POINT('Ctrl Pts',(-189.64422831163,88.2832647934035,-7.99452678846992));
#29487=CARTESIAN_POINT('Ctrl Pts',(-190.371578955361,89.2552993716194,-9.34622475164829));
#29488=CARTESIAN_POINT('Ctrl Pts',(-190.546703712354,87.0625533618215,-6.49656692485956));
#29489=CARTESIAN_POINT('Ctrl Pts',(-190.296635791104,87.4039672654561,-8.35854013664169));
#29490=CARTESIAN_POINT('Ctrl Pts',(-191.128495190513,88.4191654814962,-9.74582492495691));
#29491=CARTESIAN_POINT('Ctrl Pts',(-191.817379516886,85.2993336154583,-6.97723500735076));
#29492=CARTESIAN_POINT('Ctrl Pts',(-191.58631881165,85.6248497292438,-9.02658828514773));
#29493=CARTESIAN_POINT('Ctrl Pts',(-192.625914150862,86.721646050191,-10.4669000807354));
#29494=CARTESIAN_POINT('Ctrl Pts',(-192.445310869352,84.4074358145282,-7.19119018591865));
#29495=CARTESIAN_POINT('Ctrl Pts',(-192.223411761402,84.7247818509418,-9.32938769806592));
#29496=CARTESIAN_POINT('Ctrl Pts',(-193.36646245408,85.8602217891397,-10.7878654563762));
#29497=CARTESIAN_POINT('Ctrl Pts',(-194.304305684022,81.7033032878079,-7.77457703832778));
#29498=CARTESIAN_POINT('Ctrl Pts',(-194.121426915844,81.9789046691737,-10.1764823230672));
#29499=CARTESIAN_POINT('Ctrl Pts',(-195.560439767958,83.2403639888807,-11.66303604594));
#29500=CARTESIAN_POINT('Ctrl Pts',(-195.510473766748,79.8627399618138,-8.08647138287587));
#29501=CARTESIAN_POINT('Ctrl Pts',(-195.343662380556,80.1208834365032,-10.6467860035186));
#29502=CARTESIAN_POINT('Ctrl Pts',(-196.986083554655,81.4464501527923,-12.1309258408888));
#29503=CARTESIAN_POINT('Ctrl Pts',(-197.26422362369,77.0498973143794,-8.48148993785693));
#29504=CARTESIAN_POINT('Ctrl Pts',(-197.110469889354,77.3001806896492,-11.2686726614448));
#29505=CARTESIAN_POINT('Ctrl Pts',(-199.061639908547,78.6896512667519,-12.7235158739264));
#29506=CARTESIAN_POINT('Ctrl Pts',(-197.839595055258,76.1035745652819,-8.60067013564272));
#29507=CARTESIAN_POINT('Ctrl Pts',(-197.693451452524,76.3452591128515,-11.4629048769373));
#29508=CARTESIAN_POINT('Ctrl Pts',(-199.743053232215,77.7596906841316,-12.9023052799916));
#29509=CARTESIAN_POINT('Ctrl Pts',(-198.971269927631,74.1939245965756,-8.81827543079709));
#29510=CARTESIAN_POINT('Ctrl Pts',(-198.840144887273,74.4184120242095,-11.8283305042784));
#29511=CARTESIAN_POINT('Ctrl Pts',(-201.084141185834,75.8782216647446,-13.2287486186965));
#29512=CARTESIAN_POINT('Ctrl Pts',(-199.528026213893,73.2297480452024,-8.9167473697722));
#29513=CARTESIAN_POINT('Ctrl Pts',(-199.403933368659,73.4456397089867,-11.999284368886));
#29514=CARTESIAN_POINT('Ctrl Pts',(-201.744353740694,74.9258683491321,-13.3764727664485));
#29515=CARTESIAN_POINT('Ctrl Pts',(-201.161792437304,70.3249942677904,-9.18473475784064));
#29516=CARTESIAN_POINT('Ctrl Pts',(-201.069113535252,70.4962985183013,-12.4841466691128));
#29517=CARTESIAN_POINT('Ctrl Pts',(-203.682864677576,72.0498212174151,-13.7784991672417));
#29518=CARTESIAN_POINT('Ctrl Pts',(-202.204497602129,68.3686954361411,-9.327550429722));
#29519=CARTESIAN_POINT('Ctrl Pts',(-202.122699464231,68.5235270163752,-12.7632527718059));
#29520=CARTESIAN_POINT('Ctrl Pts',(-204.921631000465,70.1037195380372,-13.9927475603924));
#29521=CARTESIAN_POINT('Ctrl Pts',(-204.197844600951,64.4174374747376,-9.56200891039826));
#29522=CARTESIAN_POINT('Ctrl Pts',(-204.139132956947,64.5385208888658,-13.2647553306726));
#29523=CARTESIAN_POINT('Ctrl Pts',(-207.292248848856,66.1565464226095,-14.3444784427628));
#29524=CARTESIAN_POINT('Ctrl Pts',(-205.148489282526,62.4224747699383,-9.6535097636974));
#29525=CARTESIAN_POINT('Ctrl Pts',(-205.098222238211,62.5281076726303,-13.4851030107949));
#29526=CARTESIAN_POINT('Ctrl Pts',(-208.424103723681,64.1554710849893,-14.4817477042882));
#29527=CARTESIAN_POINT('Ctrl Pts',(-207.863010265155,56.3804553729788,-9.87162265399631));
#29528=CARTESIAN_POINT('Ctrl Pts',(-207.874530509962,56.3622740214675,-14.0896831956044));
#29529=CARTESIAN_POINT('Ctrl Pts',(-211.659039648998,58.0728675461335,-14.8089642189829));
#29530=CARTESIAN_POINT('Ctrl Pts',(-209.489746376511,52.2763554538315,-9.94272550904972));
#29531=CARTESIAN_POINT('Ctrl Pts',(-209.500567148536,52.239261066085,-14.3961534366159));
#29532=CARTESIAN_POINT('Ctrl Pts',(-213.601767269327,53.9120928346637,-14.9156391942734));
#29533=CARTESIAN_POINT('Ctrl Pts',(-211.653837598457,46.0069427729526,-9.99217179438664));
#29534=CARTESIAN_POINT('Ctrl Pts',(-211.654748063316,46.0028378682449,-14.7791601532076));
#29535=CARTESIAN_POINT('Ctrl Pts',(-216.189589140866,47.5215622113001,-14.9898323220643));
#29536=CARTESIAN_POINT('Ctrl Pts',(-212.329136320276,43.8982352536057,-9.99883253041345));
#29537=CARTESIAN_POINT('Ctrl Pts',(-212.331887292226,43.8852959564764,-14.8942914798601));
#29538=CARTESIAN_POINT('Ctrl Pts',(-216.99775401071,45.3664543056449,-14.99982994474));
#29539=CARTESIAN_POINT('Ctrl Pts',(-213.586563915695,39.6427642163839,-9.99904901899915));
#29540=CARTESIAN_POINT('Ctrl Pts',(-213.594819890769,39.6109883608531,-15.1032774268557));
#29541=CARTESIAN_POINT('Ctrl Pts',(-218.503477700196,41.0074627753361,-15.0001657416214));
#29542=CARTESIAN_POINT('Ctrl Pts',(-214.169149505489,37.4941453785589,-9.99258591104121));
#29543=CARTESIAN_POINT('Ctrl Pts',(-214.177547647221,37.4569157620953,-15.1964629582924));
#29544=CARTESIAN_POINT('Ctrl Pts',(-219.201583812779,38.8016704170055,-14.99047558146));
#29545=CARTESIAN_POINT('Ctrl Pts',(-215.771854048122,31.0022455423769,-9.96182684240677));
#29546=CARTESIAN_POINT('Ctrl Pts',(-215.799160452695,30.8835450730081,-15.4509064845787));
#29547=CARTESIAN_POINT('Ctrl Pts',(-221.123034242247,32.1244801171726,-14.9443482381631));
#29548=CARTESIAN_POINT('Ctrl Pts',(-216.636779994235,26.656889293641,-9.92696752601132));
#29549=CARTESIAN_POINT('Ctrl Pts',(-216.651517550254,26.5601579572741,-15.5778765399567));
#29550=CARTESIAN_POINT('Ctrl Pts',(-222.161298573218,27.6385960407911,-14.8920638015871));
#29551=CARTESIAN_POINT('Ctrl Pts',(-217.971708585098,17.9323050948719,-9.86264007720543));
#29552=CARTESIAN_POINT('Ctrl Pts',(-217.98395218067,17.8351858692922,-15.7751687151717));
#29553=CARTESIAN_POINT('Ctrl Pts',(-223.764494274026,18.6116604334835,-14.7955788665586));
#29554=CARTESIAN_POINT('Ctrl Pts',(-218.441684997606,13.5530627335445,-9.83311016810406));
#29555=CARTESIAN_POINT('Ctrl Pts',(-218.444591836418,13.4953035845419,-15.8420879379444));
#29556=CARTESIAN_POINT('Ctrl Pts',(-224.3293991122,14.0705718828394,-14.7512857241696));
#29557=CARTESIAN_POINT('Ctrl Pts',(-218.98892491974,4.76083842406514,-9.79797621148514));
#29558=CARTESIAN_POINT('Ctrl Pts',(-218.989185405442,4.72249428361865,-15.9213704338492));
#29559=CARTESIAN_POINT('Ctrl Pts',(-224.987222679375,4.94518643901801,-14.6985866952544));
#29560=CARTESIAN_POINT('Ctrl Pts',(-219.066199483219,0.347844039587536,
-9.79239498047612));
#29561=CARTESIAN_POINT('Ctrl Pts',(-219.064738571508,0.358452420802183,
-15.9323153280885));
#29562=CARTESIAN_POINT('Ctrl Pts',(-225.08015488072,0.360857152534145,-14.6902150849217));
#29563=CARTESIAN_POINT('Ctrl Pts',(-218.882089664708,-6.29742822354361,
-9.80469739981719));
#29564=CARTESIAN_POINT('Ctrl Pts',(-218.881384487388,-6.27783716390587,
-15.9056638247615));
#29565=CARTESIAN_POINT('Ctrl Pts',(-224.858807959456,-6.53966795784784,
-14.7086681091492));
#29566=CARTESIAN_POINT('Ctrl Pts',(-218.770640597971,-8.5168252216966,-9.81212408241458));
#29567=CARTESIAN_POINT('Ctrl Pts',(-218.77099042416,-8.48718110804912,-15.8896189712452));
#29568=CARTESIAN_POINT('Ctrl Pts',(-224.724819198552,-8.84385385870031,
-14.7198077601516));
#29569=CARTESIAN_POINT('Ctrl Pts',(-218.445706585932,-12.9643846257828,
-9.83258697597486));
#29570=CARTESIAN_POINT('Ctrl Pts',(-218.447558735051,-12.9256116392978,
-15.8424934042915));
#29571=CARTESIAN_POINT('Ctrl Pts',(-224.334251471307,-13.4588585853863,
-14.7505009402079));
#29572=CARTESIAN_POINT('Ctrl Pts',(-218.233279978387,-15.1775360624383,
-9.84554950482581));
#29573=CARTESIAN_POINT('Ctrl Pts',(-218.236862025186,-15.1309441945871,
-15.8117609314217));
#29574=CARTESIAN_POINT('Ctrl Pts',(-224.078945146157,-15.754094702541,-14.769943939359));
#29575=CARTESIAN_POINT('Ctrl Pts',(-217.44965178097,-21.7782118624344,-9.88922208942823));
#29576=CARTESIAN_POINT('Ctrl Pts',(-217.459829407993,-21.6907915561905,
-15.6977966994989));
#29577=CARTESIAN_POINT('Ctrl Pts',(-223.13742499135,-22.5936734469255,-14.8354495694809));
#29578=CARTESIAN_POINT('Ctrl Pts',(-216.732153346241,-26.1303721630048,
-9.92513272450046));
#29579=CARTESIAN_POINT('Ctrl Pts',(-216.753951919438,-26.0158068183044,
-15.5940689166965));
#29580=CARTESIAN_POINT('Ctrl Pts',(-222.275639117307,-27.0954312018765,
-14.8893122662313));
#29581=CARTESIAN_POINT('Ctrl Pts',(-214.915312965014,-34.7401291355706,
-9.98260167196437));
#29582=CARTESIAN_POINT('Ctrl Pts',(-214.935762892442,-34.6425169654146,
-15.3168242444749));
#29583=CARTESIAN_POINT('Ctrl Pts',(-220.095831592936,-35.9737986453296,
-14.975504791654));
#29584=CARTESIAN_POINT('Ctrl Pts',(-213.815951507118,-38.997732367201,-10.0042638421583));
#29585=CARTESIAN_POINT('Ctrl Pts',(-213.847033440636,-38.893318416415,-15.1477002122303));
#29586=CARTESIAN_POINT('Ctrl Pts',(-218.777784106532,-40.3504347492802,
-15.0079905031581));
#29587=CARTESIAN_POINT('Ctrl Pts',(-211.234344254847,-47.4180803462803,
-9.99138542271174));
#29588=CARTESIAN_POINT('Ctrl Pts',(-211.252009920408,-47.3564561926427,
-14.7119977239021));
#29589=CARTESIAN_POINT('Ctrl Pts',(-215.687315361276,-48.9667036279376,
-14.9886489895387));
#29590=CARTESIAN_POINT('Ctrl Pts',(-209.75211504862,-51.5808392384507,-9.95731237985128));
#29591=CARTESIAN_POINT('Ctrl Pts',(-209.774784444065,-51.529992979264,-14.4524533619249));
#29592=CARTESIAN_POINT('Ctrl Pts',(-213.914906046157,-53.206374129089,-14.9375236211255));
#29593=CARTESIAN_POINT('Ctrl Pts',(-207.233810470461,-57.7518422440691,
-9.8166773227685));
#29594=CARTESIAN_POINT('Ctrl Pts',(-207.20309976548,-57.8216061018363,-13.9396592655048));
#29595=CARTESIAN_POINT('Ctrl Pts',(-210.909503771198,-59.4516238932021,
-14.7265343478991));
#29596=CARTESIAN_POINT('Ctrl Pts',(-206.343367468842,-59.8001282170186,
-9.75447731805782));
#29597=CARTESIAN_POINT('Ctrl Pts',(-206.306005665109,-59.8842764834739,
-13.7521834792451));
#29598=CARTESIAN_POINT('Ctrl Pts',(-209.847720713297,-61.5177848329008,
-14.6332201986806));
#29599=CARTESIAN_POINT('Ctrl Pts',(-204.476765026371,-63.8405295173718,
-9.58938895529315));
#29600=CARTESIAN_POINT('Ctrl Pts',(-204.419864648177,-63.9571626937035,
-13.329314053494));
#29601=CARTESIAN_POINT('Ctrl Pts',(-207.624289029391,-65.5783610758614,
-14.3855537798929));
#29602=CARTESIAN_POINT('Ctrl Pts',(-203.49960767437,-65.8355428611045,-9.48655973173275));
#29603=CARTESIAN_POINT('Ctrl Pts',(-203.433512500785,-65.968284694467,-13.0953532628466));
#29604=CARTESIAN_POINT('Ctrl Pts',(-206.461446708194,-67.5757325777054,
-14.2312904187871));
#29605=CARTESIAN_POINT('Ctrl Pts',(-201.45887205873,-69.7747638156398,-9.22591935843988));
#29606=CARTESIAN_POINT('Ctrl Pts',(-201.368484720857,-69.941659180332,-12.5633651459106));
#29607=CARTESIAN_POINT('Ctrl Pts',(-204.03575029879,-71.5029679315967,-13.8402831180884));
#29608=CARTESIAN_POINT('Ctrl Pts',(-200.395284333713,-71.7189792947419,
-9.06826475769951));
#29609=CARTESIAN_POINT('Ctrl Pts',(-200.2932655858,-71.90279735052,-12.2674645147884));
#29610=CARTESIAN_POINT('Ctrl Pts',(-202.772885289101,-73.432839265888,-13.6037743174855));
#29611=CARTESIAN_POINT('Ctrl Pts',(-198.18283411717,-75.5555694788219,-8.67680237261049));
#29612=CARTESIAN_POINT('Ctrl Pts',(-198.051808705163,-75.7741525073902,
-11.5869496831444));
#29613=CARTESIAN_POINT('Ctrl Pts',(-200.149286733965,-77.222776724018,-13.0165160576299));
#29614=CARTESIAN_POINT('Ctrl Pts',(-197.033949531596,-77.4479653439144,
-8.44340981108465));
#29615=CARTESIAN_POINT('Ctrl Pts',(-196.888887581277,-77.6837498187098,
-11.205475577738));
#29616=CARTESIAN_POINT('Ctrl Pts',(-198.788527494164,-79.0828624701376,
-12.6663899188091));
#29617=CARTESIAN_POINT('Ctrl Pts',(-195.247729756749,-80.2461536453752,
-8.00941135562084));
#29618=CARTESIAN_POINT('Ctrl Pts',(-195.066101080631,-80.5254857528079,
-10.530388667617));
#29619=CARTESIAN_POINT('Ctrl Pts',(-196.6758925451,-81.8181682371439,-12.0153234692363));
#29620=CARTESIAN_POINT('Ctrl Pts',(-194.6416840559,-81.1723200972973,-7.85053644481165));
#29621=CARTESIAN_POINT('Ctrl Pts',(-194.451609817737,-81.4601421251086,
-10.2906945195429));
#29622=CARTESIAN_POINT('Ctrl Pts',(-195.959582481097,-82.7209577867424,
-11.7769863872961));
#29623=CARTESIAN_POINT('Ctrl Pts',(-193.414428959512,-83.0027585457057,
-7.49863868716929));
#29624=CARTESIAN_POINT('Ctrl Pts',(-193.206673895877,-83.3072532983952,
-9.77173373334771));
#29625=CARTESIAN_POINT('Ctrl Pts',(-194.510093498015,-84.4999373718914,
-11.2490853481395));
#29626=CARTESIAN_POINT('Ctrl Pts',(-192.792617590937,-83.9079862550153,
-7.30555612066123));
#29627=CARTESIAN_POINT('Ctrl Pts',(-192.575907971764,-84.2208076263337,
-9.49288654034082));
#29628=CARTESIAN_POINT('Ctrl Pts',(-193.776202443296,-85.3770629978107,
-10.9594318944836));
#29629=CARTESIAN_POINT('Ctrl Pts',(-191.534262284156,-85.6970547926546,
-6.87464494826575));
#29630=CARTESIAN_POINT('Ctrl Pts',(-191.298951356079,-86.0260858611082,
-8.8826451632366));
#29631=CARTESIAN_POINT('Ctrl Pts',(-192.292150323284,-87.1051898982516,
-10.3129993370047));
#29632=CARTESIAN_POINT('Ctrl Pts',(-190.897692592206,-86.5809228644259,
-6.63700227874789));
#29633=CARTESIAN_POINT('Ctrl Pts',(-190.652958604134,-86.9180526562817,
-8.55216637333298));
#29634=CARTESIAN_POINT('Ctrl Pts',(-191.541959253817,-87.9562162178622,
-9.95649928586201));
#29635=CARTESIAN_POINT('Ctrl Pts',(-189.584682347239,-88.3624698219694,
-6.08799905112524));
#29636=CARTESIAN_POINT('Ctrl Pts',(-189.320453977114,-88.7150993305577,
-7.80170139306956));
#29637=CARTESIAN_POINT('Ctrl Pts',(-189.995794337287,-89.6659208608691,
-9.13291138381351));
#29638=CARTESIAN_POINT('Ctrl Pts',(-188.907584299326,-89.2592395987802,
-5.77452884411308));
#29639=CARTESIAN_POINT('Ctrl Pts',(-188.633022709524,-89.6201125002178,
-7.38005660091507));
#29640=CARTESIAN_POINT('Ctrl Pts',(-189.199000170436,-90.5235796561882,
-8.66259199213005));
#29641=CARTESIAN_POINT('Ctrl Pts',(-188.226751608154,-90.1401577923431,
-5.4077170003843));
#29642=CARTESIAN_POINT('Ctrl Pts',(-187.93744048601,-90.5142672861031,-6.89114911006534));
#29643=CARTESIAN_POINT('Ctrl Pts',(-188.39869005518,-91.362817758299,-8.1123941340948));
#29644=CARTESIAN_POINT('Origin',(-71.5953323638214,6.93889390390723E-15,
-26.5));
#29645=CARTESIAN_POINT('Ctrl Pts',(-188.850942384682,90.9673968784446,5.31766757924555));
#29646=CARTESIAN_POINT('Ctrl Pts',(-189.341118335966,90.3355674301194,5.58646961538285));
#29647=CARTESIAN_POINT('Ctrl Pts',(-189.830924097054,89.6936385792413,5.82722845321623));
#29648=CARTESIAN_POINT('Ctrl Pts',(-190.318786696358,89.0431674195335,6.04773461915937));
#29649=CARTESIAN_POINT('Ctrl Pts',(-190.482667264906,88.8246641285877,6.1218060398724));
#29650=CARTESIAN_POINT('Ctrl Pts',(-190.646328518149,88.6051970380796,6.19359259998661));
#29651=CARTESIAN_POINT('Ctrl Pts',(-190.809710697124,88.3848254779465,6.2633908242173));
#29652=CARTESIAN_POINT('Ctrl Pts',(-190.810466894386,88.3838055113162,6.26371387797037));
#29653=CARTESIAN_POINT('Ctrl Pts',(-190.811223085654,88.3827855253331,6.26403688911534));
#29654=CARTESIAN_POINT('Ctrl Pts',(-190.81197927092,88.3817655200031,6.26435985768164));
#29655=CARTESIAN_POINT('Ctrl Pts',(-191.415025663252,87.5683265894712,6.5219224384322));
#29656=CARTESIAN_POINT('Ctrl Pts',(-192.014372732003,86.7424513122927,6.75185269721188));
#29657=CARTESIAN_POINT('Ctrl Pts',(-192.608472917412,85.9055593357088,6.96149402186932));
#29658=CARTESIAN_POINT('Ctrl Pts',(-192.653739491705,85.8417936043329,6.97746732878041));
#29659=CARTESIAN_POINT('Ctrl Pts',(-192.698975604839,85.7779639226609,6.99332287300553));
#29660=CARTESIAN_POINT('Ctrl Pts',(-192.74418057204,85.7140709218425,7.00906391406534));
#29661=CARTESIAN_POINT('Ctrl Pts',(-192.745135383982,85.7127213843022,7.00939639376675));
#29662=CARTESIAN_POINT('Ctrl Pts',(-192.746090182109,85.7113718184013,7.00972882239919));
#29663=CARTESIAN_POINT('Ctrl Pts',(-192.747044966413,85.7100222241461,7.01006119999323));
#29664=CARTESIAN_POINT('Ctrl Pts',(-193.340906354287,84.8705950215575,7.21679503344427));
#29665=CARTESIAN_POINT('Ctrl Pts',(-193.930245240205,84.0189651457988,7.40382485455509));
#29666=CARTESIAN_POINT('Ctrl Pts',(-194.511008670157,83.1605775933826,7.57462063256265));
#29667=CARTESIAN_POINT('Ctrl Pts',(-194.554435141729,83.0963918325032,7.58739185336559));
#29668=CARTESIAN_POINT('Ctrl Pts',(-194.597813668124,83.0321683003785,7.60007232470945));
#29669=CARTESIAN_POINT('Ctrl Pts',(-194.641142556604,82.9679092789718,7.61266350630674));
#29670=CARTESIAN_POINT('Ctrl Pts',(-194.64192321951,82.9667515148069,7.61289036346279));
#29671=CARTESIAN_POINT('Ctrl Pts',(-194.642703866312,82.9655937391075,7.61311719163327));
#29672=CARTESIAN_POINT('Ctrl Pts',(-194.643484497,82.9644359518865,7.6133439908268));
#29673=CARTESIAN_POINT('Ctrl Pts',(-195.26639704584,82.0405673424527,7.79432081605224));
#29674=CARTESIAN_POINT('Ctrl Pts',(-195.879202354609,81.109240118497,7.95688686492277));
#29675=CARTESIAN_POINT('Ctrl Pts',(-196.481682775292,80.1707231918713,8.10499840407016));
#29676=CARTESIAN_POINT('Ctrl Pts',(-196.482156857174,80.1699846884177,8.10511495059168));
#29677=CARTESIAN_POINT('Ctrl Pts',(-196.482630932664,80.1692461805125,8.10523148816305));
#29678=CARTESIAN_POINT('Ctrl Pts',(-196.48310500176,80.1685076681557,8.10534801678623));
#29679=CARTESIAN_POINT('Ctrl Pts',(-197.688784784991,78.2902805809609,8.40171031118339));
#29680=CARTESIAN_POINT('Ctrl Pts',(-198.853091809375,76.3833019518293,8.64076529068621));
#29681=CARTESIAN_POINT('Ctrl Pts',(-199.974927008656,74.4488082848391,8.84133536347261));
#29682=CARTESIAN_POINT('Ctrl Pts',(-199.975191724801,74.4483518080694,8.8413826914016));
#29683=CARTESIAN_POINT('Ctrl Pts',(-199.975456438584,74.4478953297663,8.84143001716346));
#29684=CARTESIAN_POINT('Ctrl Pts',(-199.975721150003,74.4474388499298,8.84147734075833));
#29685=CARTESIAN_POINT('Ctrl Pts',(-201.097094425615,72.5136942047661,9.04195004698192));
#29686=CARTESIAN_POINT('Ctrl Pts',(-202.176057085258,70.5524290707013,9.2035344356386));
#29687=CARTESIAN_POINT('Ctrl Pts',(-203.211775255623,68.564256990898,9.33720992260623));
#29688=CARTESIAN_POINT('Ctrl Pts',(-203.212835287712,68.5622221456433,9.33734673618142));
#29689=CARTESIAN_POINT('Ctrl Pts',(-203.213895274515,68.5601872721942,9.33748352035168));
#29690=CARTESIAN_POINT('Ctrl Pts',(-203.21495521603,68.5581523705511,9.33762027512486));
#29691=CARTESIAN_POINT('Ctrl Pts',(-204.249652408617,66.5717153948246,9.47111799919037));
#29692=CARTESIAN_POINT('Ctrl Pts',(-205.241200921077,64.5583939991535,9.57660331773388));
#29693=CARTESIAN_POINT('Ctrl Pts',(-206.188735439408,62.5184870637267,9.66139767362455));
#29694=CARTESIAN_POINT('Ctrl Pts',(-206.19056002032,62.5145590007537,9.66156095439187));
#29695=CARTESIAN_POINT('Ctrl Pts',(-206.192384445048,62.5106308228101,9.66172415830768));
#29696=CARTESIAN_POINT('Ctrl Pts',(-206.194208713484,62.5067025301279,9.66188728540609));
#29697=CARTESIAN_POINT('Ctrl Pts',(-206.666525419703,61.4896382516984,9.7041221080299));
#29698=CARTESIAN_POINT('Ctrl Pts',(-207.128379381789,60.4648516858952,9.74120877012034));
#29699=CARTESIAN_POINT('Ctrl Pts',(-207.577897027375,59.4364154683561,9.77373815047265));
#29700=CARTESIAN_POINT('Ctrl Pts',(-207.580068445556,59.431447554144,9.77389528532283));
#29701=CARTESIAN_POINT('Ctrl Pts',(-207.582239572049,59.4264795655298,9.77405231379252));
#29702=CARTESIAN_POINT('Ctrl Pts',(-207.584410406868,59.4215115025229,9.77420923596013));
#29703=CARTESIAN_POINT('Ctrl Pts',(-208.033367357209,58.3940512842233,9.80666278664411));
#29704=CARTESIAN_POINT('Ctrl Pts',(-208.469851754248,57.3634026279674,9.83457096111565));
#29705=CARTESIAN_POINT('Ctrl Pts',(-208.893990826528,56.3295993288226,9.85862681314411));
#29706=CARTESIAN_POINT('Ctrl Pts',(-208.896457271165,56.3235875775624,9.85876670223024));
#29707=CARTESIAN_POINT('Ctrl Pts',(-208.898923299152,56.3175757198386,9.8589064637187));
#29708=CARTESIAN_POINT('Ctrl Pts',(-208.901388910506,56.3115637556553,9.85904609770791));
#29709=CARTESIAN_POINT('Ctrl Pts',(-210.603104765652,52.1622258018391,9.95541869631808));
#29710=CARTESIAN_POINT('Ctrl Pts',(-212.106358542097,47.9621739982348,9.99108073365087));
#29711=CARTESIAN_POINT('Ctrl Pts',(-213.416141475183,43.7127381801167,9.99852944383294));
#29712=CARTESIAN_POINT('Ctrl Pts',(-213.419320039466,43.7024257042292,9.99854752026648));
#29713=CARTESIAN_POINT('Ctrl Pts',(-213.422497464223,43.6921129374695,9.99856542770493));
#29714=CARTESIAN_POINT('Ctrl Pts',(-213.425673749455,43.6817998798392,9.99858316645284));
#29715=CARTESIAN_POINT('Ctrl Pts',(-214.733236103275,39.4362850960293,10.0058855707623));
#29716=CARTESIAN_POINT('Ctrl Pts',(-215.847686530337,35.1414767092267,9.98461098471693));
#29717=CARTESIAN_POINT('Ctrl Pts',(-216.769233470622,30.7974644027352,9.95600465872816));
#29718=CARTESIAN_POINT('Ctrl Pts',(-216.772375208496,30.7826547957672,9.9559071340402));
#29719=CARTESIAN_POINT('Ctrl Pts',(-216.775514704529,30.7678446169708,9.95580952290657));
#29720=CARTESIAN_POINT('Ctrl Pts',(-216.778651958541,30.7530338663012,9.95571182588763));
#29721=CARTESIAN_POINT('Ctrl Pts',(-217.69798150674,26.4129451558353,9.92708304545502));
#29722=CARTESIAN_POINT('Ctrl Pts',(-218.424787910683,22.0237499448137,9.89108693511256));
#29723=CARTESIAN_POINT('Ctrl Pts',(-218.954543661828,17.5843174969628,9.86183278666612));
#29724=CARTESIAN_POINT('Ctrl Pts',(-218.956871344149,17.5648111708836,9.86170424749687));
#29725=CARTESIAN_POINT('Ctrl Pts',(-218.959195214687,17.5453038729898,9.86157582861175));
#29726=CARTESIAN_POINT('Ctrl Pts',(-218.961515272787,17.5257956031157,9.86144753085713));
#29727=CARTESIAN_POINT('Ctrl Pts',(-219.091650787911,16.4315476833897,9.85425111866854));
#29728=CARTESIAN_POINT('Ctrl Pts',(-219.209795922764,15.3341948244095,9.84743578264517));
#29729=CARTESIAN_POINT('Ctrl Pts',(-219.31582170744,14.2338471358419,9.84115131033219));
#29730=CARTESIAN_POINT('Ctrl Pts',(-219.317817511001,14.2131344588084,9.84103301295519));
#29731=CARTESIAN_POINT('Ctrl Pts',(-219.31980905213,14.192420238668,9.84091490168962));
#29732=CARTESIAN_POINT('Ctrl Pts',(-219.321796327431,14.1717045123362,9.84079697751308));
#29733=CARTESIAN_POINT('Ctrl Pts',(-219.427264023453,13.0722896869807,9.83453856369359));
#29734=CARTESIAN_POINT('Ctrl Pts',(-219.520734074763,11.9684395739338,9.82880673133093));
#29735=CARTESIAN_POINT('Ctrl Pts',(-219.601691870632,10.8656763132971,9.82374740145546));
#29736=CARTESIAN_POINT('Ctrl Pts',(-219.603297940124,10.8437993042859,9.82364703267349));
#29737=CARTESIAN_POINT('Ctrl Pts',(-219.604899106509,10.8219226927283,9.82354693073774));
#29738=CARTESIAN_POINT('Ctrl Pts',(-219.606495370559,10.8000464796908,9.82344709613719));
#29739=CARTESIAN_POINT('Ctrl Pts',(-219.768858415878,8.5749205235309,9.81329247931069));
#29740=CARTESIAN_POINT('Ctrl Pts',(-219.880517558162,6.35371483186536,9.80590845216625));
#29741=CARTESIAN_POINT('Ctrl Pts',(-219.942344006131,4.13636470843061,9.80180544072015));
#29742=CARTESIAN_POINT('Ctrl Pts',(-219.943012881674,4.11237608680465,9.801761051885));
#29743=CARTESIAN_POINT('Ctrl Pts',(-219.943675933535,4.08838791580208,9.8017170610927));
#29744=CARTESIAN_POINT('Ctrl Pts',(-219.944333162218,4.06440019538434,9.80167346805754));
#29745=CARTESIAN_POINT('Ctrl Pts',(-220.066370321029,-0.389746924528067,
9.79357891848717));
#29746=CARTESIAN_POINT('Ctrl Pts',(-219.987631786347,-4.82836129360515,
9.79922661021772));
#29747=CARTESIAN_POINT('Ctrl Pts',(-219.711339275957,-9.25169566130756,
9.81683113342425));
#29748=CARTESIAN_POINT('Ctrl Pts',(-219.709579972076,-9.27986142413934,
9.81694323094711));
#29749=CARTESIAN_POINT('Ctrl Pts',(-219.707812658021,-9.30802656742054,
9.81705581248959));
#29750=CARTESIAN_POINT('Ctrl Pts',(-219.706037333374,-9.3361910911259,9.81716887563367));
#29751=CARTESIAN_POINT('Ctrl Pts',(-219.427502399894,-13.7549906314892,
9.83490762294272));
#29752=CARTESIAN_POINT('Ctrl Pts',(-218.951784949751,-18.1585397204247,
9.86451878801393));
#29753=CARTESIAN_POINT('Ctrl Pts',(-218.277266277532,-22.5467434353284,
9.89667505290868));
#29754=CARTESIAN_POINT('Ctrl Pts',(-218.272304508842,-22.579023122596,9.89691159483835));
#29755=CARTESIAN_POINT('Ctrl Pts',(-218.267331966596,-22.6113019783348,
9.89714824949614));
#29756=CARTESIAN_POINT('Ctrl Pts',(-218.262348648669,-22.6435800023996,
9.8973850108931));
#29757=CARTESIAN_POINT('Ctrl Pts',(-217.926448866683,-24.8192752731317,
9.91334387661025));
#29758=CARTESIAN_POINT('Ctrl Pts',(-217.541590744706,-26.9911917525532,
9.92978970018313));
#29759=CARTESIAN_POINT('Ctrl Pts',(-217.107123822393,-29.1592853602726,
9.94488796227917));
#29760=CARTESIAN_POINT('Ctrl Pts',(-217.100247949909,-29.1935976045774,
9.94512690733937));
#29761=CARTESIAN_POINT('Ctrl Pts',(-217.093359647348,-29.2279088910387,
9.94536550728949));
#29762=CARTESIAN_POINT('Ctrl Pts',(-217.086458911175,-29.2622192194123,
9.94560375335194));
#29763=CARTESIAN_POINT('Ctrl Pts',(-216.872106429072,-30.3279756639031,
9.95300421520923));
#29764=CARTESIAN_POINT('Ctrl Pts',(-216.645741368245,-31.3928784273454,
9.96006389214994));
#29765=CARTESIAN_POINT('Ctrl Pts',(-216.407304521944,-32.4567111069465,
9.96651848904424));
#29766=CARTESIAN_POINT('Ctrl Pts',(-216.399387998386,-32.4920322269846,
9.96673279303779));
#29767=CARTESIAN_POINT('Ctrl Pts',(-216.391457819029,-32.5273535271178,
9.96694643567054));
#29768=CARTESIAN_POINT('Ctrl Pts',(-216.383514027764,-32.5626748172608,
9.96715940532502));
#29769=CARTESIAN_POINT('Ctrl Pts',(-216.144496659423,-33.6254421451658,
9.97356735898984));
#29770=CARTESIAN_POINT('Ctrl Pts',(-215.893087346094,-34.6884985009459,
9.9793701644089));
#29771=CARTESIAN_POINT('Ctrl Pts',(-215.630475785694,-35.7466478938294,
9.98424576551855));
#29772=CARTESIAN_POINT('Ctrl Pts',(-215.621483320461,-35.7828815295937,
9.98441271808302));
#29773=CARTESIAN_POINT('Ctrl Pts',(-215.612477740882,-35.8191096434725,
9.98457862995805));
#29774=CARTESIAN_POINT('Ctrl Pts',(-215.603459052608,-35.8553322274098,
9.98474348708846));
#29775=CARTESIAN_POINT('Ctrl Pts',(-214.523945905845,-40.19107977512,10.0044764498213));
#29776=CARTESIAN_POINT('Ctrl Pts',(-213.25628871331,-44.4489165154168,10.0091772927501));
#29777=CARTESIAN_POINT('Ctrl Pts',(-211.806023480029,-48.6303143412221,
9.97506610014392));
#29778=CARTESIAN_POINT('Ctrl Pts',(-211.792493566962,-48.6693237222522,
9.97474786768549));
#29779=CARTESIAN_POINT('Ctrl Pts',(-211.778947757168,-48.708326450718,9.9744263118785));
#29780=CARTESIAN_POINT('Ctrl Pts',(-211.765386051776,-48.7473225261173,
9.97410140367428));
#29781=CARTESIAN_POINT('Ctrl Pts',(-210.3130864592,-52.9233448463522,9.93930754560066));
#29782=CARTESIAN_POINT('Ctrl Pts',(-208.67849395231,-57.0230760419839,9.86612985349125));
#29783=CARTESIAN_POINT('Ctrl Pts',(-206.863010141496,-61.0458903190202,
9.71890425900672));
#29784=CARTESIAN_POINT('Ctrl Pts',(-206.844340078596,-61.0872601154014,
9.71739022120968));
#29785=CARTESIAN_POINT('Ctrl Pts',(-206.825650859292,-61.1286217636414,
9.71586826024716));
#29786=CARTESIAN_POINT('Ctrl Pts',(-206.80694248212,-61.1699752611634,9.71433831653629));
#29787=CARTESIAN_POINT('Ctrl Pts',(-205.90751707084,-63.1580892582013,9.64078462244658));
#29788=CARTESIAN_POINT('Ctrl Pts',(-204.963811205864,-65.1273654886791,
9.54879048714052));
#29789=CARTESIAN_POINT('Ctrl Pts',(-203.975665504039,-67.0775131761083,
9.43173502720273));
#29790=CARTESIAN_POINT('Ctrl Pts',(-202.966926805213,-69.0683020214223,
9.31224012667321));
#29791=CARTESIAN_POINT('Ctrl Pts',(-201.911874129873,-71.0391603800216,
9.16677547320627));
#29792=CARTESIAN_POINT('Ctrl Pts',(-200.810136447587,-72.9895868038661,
8.98489141523638));
#29793=CARTESIAN_POINT('Ctrl Pts',(-200.785750305287,-73.0327580388001,
8.98086554719985));
#29794=CARTESIAN_POINT('Ctrl Pts',(-200.761341285003,-73.0759192572446,
8.97682171266042));
#29795=CARTESIAN_POINT('Ctrl Pts',(-200.73690938147,-73.1190704516511,8.97275974828342));
#29796=CARTESIAN_POINT('Ctrl Pts',(-200.209418061294,-74.0507162595116,
8.88506085290961));
#29797=CARTESIAN_POINT('Ctrl Pts',(-199.671247876679,-74.9777097146329,
8.78891298975294));
#29798=CARTESIAN_POINT('Ctrl Pts',(-199.122382643862,-75.899913195448,8.68267567009917));
#29799=CARTESIAN_POINT('Ctrl Pts',(-199.09648849205,-75.9434205548256,8.67766364689428));
#29800=CARTESIAN_POINT('Ctrl Pts',(-199.070569960254,-75.9869180195701,
8.67262900795918));
#29801=CARTESIAN_POINT('Ctrl Pts',(-199.04462738396,-76.0304050557256,8.66757160750338));
#29802=CARTESIAN_POINT('Ctrl Pts',(-198.495170194593,-76.9514494573883,
8.56045714791773));
#29803=CARTESIAN_POINT('Ctrl Pts',(-197.934867869998,-77.8679119426739,
8.4431542477302));
#29804=CARTESIAN_POINT('Ctrl Pts',(-197.366984648206,-78.774595256871,8.31422453249778));
#29805=CARTESIAN_POINT('Ctrl Pts',(-197.339723045589,-78.8181211778033,
8.30803517784311));
#29806=CARTESIAN_POINT('Ctrl Pts',(-197.312442324506,-78.8616273411525,
8.3018195528268));
#29807=CARTESIAN_POINT('Ctrl Pts',(-197.285142554208,-78.9051136828285,
8.29557729592201));
#29808=CARTESIAN_POINT('Ctrl Pts',(-196.511404555994,-80.137616176096,8.11865744241741));
#29809=CARTESIAN_POINT('Ctrl Pts',(-195.722291287618,-81.3543114637074,
7.9204388246629));
#29810=CARTESIAN_POINT('Ctrl Pts',(-194.919125290429,-82.5541339329256,
7.6927527053575));
#29811=CARTESIAN_POINT('Ctrl Pts',(-194.513820130131,-83.1596055787834,
7.57785446588325));
#29812=CARTESIAN_POINT('Ctrl Pts',(-194.104936475455,-83.7607805724009,
7.4554528637455));
#29813=CARTESIAN_POINT('Ctrl Pts',(-193.692644953243,-84.357522691569,7.32450325257206));
#29814=CARTESIAN_POINT('Ctrl Pts',(-193.663328910817,-84.3999541177332,
7.31519206340129));
#29815=CARTESIAN_POINT('Ctrl Pts',(-193.633995705816,-84.4423630558444,
7.30583712450649));
#29816=CARTESIAN_POINT('Ctrl Pts',(-193.604645446565,-84.4847494063933,
7.29643769926986));
#29817=CARTESIAN_POINT('Ctrl Pts',(-193.078197563812,-85.245022231026,7.12784268030665));
#29818=CARTESIAN_POINT('Ctrl Pts',(-192.546256337125,-85.9980368951714,
6.94500033050956));
#29819=CARTESIAN_POINT('Ctrl Pts',(-192.009466142117,-86.7431938561752,
6.74358010351907));
#29820=CARTESIAN_POINT('Ctrl Pts',(-191.933679675978,-86.8483984842011,
6.71514268540938));
#29821=CARTESIAN_POINT('Ctrl Pts',(-191.857796564122,-86.9534464826587,
6.68633503791277));
#29822=CARTESIAN_POINT('Ctrl Pts',(-191.781818629018,-87.0583361629943,
6.65714506117598));
#29823=CARTESIAN_POINT('Ctrl Pts',(-191.751898900846,-87.0996411908201,
6.64565019535609));
#29824=CARTESIAN_POINT('Ctrl Pts',(-191.721964360627,-87.1409217835338,
6.63409686904724));
#29825=CARTESIAN_POINT('Ctrl Pts',(-191.692015202936,-87.18217774886,6.62248370548136));
#29826=CARTESIAN_POINT('Ctrl Pts',(-191.195374169802,-87.8663173648707,
6.42990488203561));
#29827=CARTESIAN_POINT('Ctrl Pts',(-190.694704232015,-88.543696874684,6.22095419572538));
#29828=CARTESIAN_POINT('Ctrl Pts',(-190.190903445975,-89.2134269624852,
5.98937558717201));
#29829=CARTESIAN_POINT('Ctrl Pts',(-190.070696200683,-89.3732250635884,
5.93412075753689));
#29830=CARTESIAN_POINT('Ctrl Pts',(-189.950310726361,-89.532587696832,5.87757794136475));
#29831=CARTESIAN_POINT('Ctrl Pts',(-189.829759241515,-89.6915028144458,
5.81966261655487));
#29832=CARTESIAN_POINT('Ctrl Pts',(-189.799710055655,-89.7311146857652,
5.80522639155477));
#29833=CARTESIAN_POINT('Ctrl Pts',(-189.769650680631,-89.770698618002,5.79070392907296));
#29834=CARTESIAN_POINT('Ctrl Pts',(-189.739581445364,-89.8102542734329,
5.77609284254298));
#29835=CARTESIAN_POINT('Ctrl Pts',(-189.48051683526,-90.151050118778,5.65020951356901));
#29836=CARTESIAN_POINT('Ctrl Pts',(-189.22065314064,-90.4898340171211,5.51773372111318));
#29837=CARTESIAN_POINT('Ctrl Pts',(-188.960371102286,-90.8261693459455,
5.37721625555611));
#29838=CARTESIAN_POINT('Ctrl Pts',(-188.920798880827,-90.8773044000617,
5.35585255216331));
#29839=CARTESIAN_POINT('Ctrl Pts',(-188.881216995801,-90.9283828777641,
5.33430306200019));
#29840=CARTESIAN_POINT('Ctrl Pts',(-188.841626791297,-90.9794032692678,
5.31256280209118));
#29841=CARTESIAN_POINT('Ctrl Pts',(-188.811784559938,-91.0178613259103,
5.29617546905901));
#29842=CARTESIAN_POINT('Ctrl Pts',(-188.781930263047,-91.0562954959819,
5.27967549520592));
#29843=CARTESIAN_POINT('Ctrl Pts',(-188.752067771096,-91.094701048084,5.26306128947281));
#29844=CARTESIAN_POINT('Ctrl Pts',(-188.541474345477,-91.3655410299928,
5.14589616792414));
#29845=CARTESIAN_POINT('Ctrl Pts',(-188.330252784274,-91.6352404391924,
5.02295648219355));
#29846=CARTESIAN_POINT('Ctrl Pts',(-188.119833342626,-91.9020407097296,
4.8936803057521));
#29847=CARTESIAN_POINT('Ctrl Pts',(-188.02973359339,-92.0162822326764,4.83832538707953));
#29848=CARTESIAN_POINT('Ctrl Pts',(-187.939780930582,-92.1299923331076,
4.78180927034326));
#29849=CARTESIAN_POINT('Ctrl Pts',(-187.850087343075,-92.2430339968832,
4.72409069046544));
#29850=CARTESIAN_POINT('Ctrl Pts',(-187.820954449995,-92.2797504533881,
4.70534342811248));
#29851=CARTESIAN_POINT('Ctrl Pts',(-187.791845691714,-92.3164006214176,
4.68646975713368));
#29852=CARTESIAN_POINT('Ctrl Pts',(-187.762763236003,-92.3529821561108,
4.66746483777612));
#29853=CARTESIAN_POINT('Ctrl Pts',(-187.563248765946,-92.6039425832705,
4.53708532472098));
#29854=CARTESIAN_POINT('Ctrl Pts',(-187.364884238019,-92.8517833155242,
4.40057063569385));
#29855=CARTESIAN_POINT('Ctrl Pts',(-187.168269560478,-93.0958704985984,
4.25621167985531));
#29856=CARTESIAN_POINT('Ctrl Pts',(-187.069597876729,-93.2183664060079,
4.18376469158894));
#29857=CARTESIAN_POINT('Ctrl Pts',(-186.971366884062,-93.339917021235,4.10934282074714));
#29858=CARTESIAN_POINT('Ctrl Pts',(-186.873652225136,-93.4604426826047,
4.03273507861638));
#29859=CARTESIAN_POINT('Ctrl Pts',(-186.846241351334,-93.4942524889327,
4.01124510797255));
#29860=CARTESIAN_POINT('Ctrl Pts',(-186.818869584361,-93.5279833711846,
3.98958788461428));
#29861=CARTESIAN_POINT('Ctrl Pts',(-186.79154037738,-93.5616315776803,3.96775330026969));
#29862=CARTESIAN_POINT('Ctrl Pts',(-186.644952825736,-93.7421127826717,
3.85063763487754));
#29863=CARTESIAN_POINT('Ctrl Pts',(-186.499520947913,-93.9202997456518,
3.72843956140678));
#29864=CARTESIAN_POINT('Ctrl Pts',(-186.35585082079,-94.0955230792172,3.59967230248097));
#29865=CARTESIAN_POINT('Ctrl Pts',(-186.222513907549,-94.2581437916332,
3.48016639561181));
#29866=CARTESIAN_POINT('Ctrl Pts',(-186.090694643596,-94.4182116806052,
3.35500174419214));
#29867=CARTESIAN_POINT('Ctrl Pts',(-185.960868132876,-94.5752059646028,
3.22303145109493));
#29868=CARTESIAN_POINT('Ctrl Pts',(-185.950806964742,-94.5873725542976,
3.21280414620755));
#29869=CARTESIAN_POINT('Ctrl Pts',(-185.940757758819,-94.5995206928895,
3.202535992431));
#29870=CARTESIAN_POINT('Ctrl Pts',(-185.930720733152,-94.6116501423323,
3.19222646869787));
#29871=CARTESIAN_POINT('Ctrl Pts',(-185.906249241296,-94.6412232183741,
3.16709059334336));
#29872=CARTESIAN_POINT('Ctrl Pts',(-185.881838142642,-94.6706996607867,
3.1416885525429));
#29873=CARTESIAN_POINT('Ctrl Pts',(-185.857500658255,-94.7000641881417,
3.11601154655574));
#29874=CARTESIAN_POINT('Ctrl Pts',(-185.771154483368,-94.8042456464287,
3.0249129262427));
#29875=CARTESIAN_POINT('Ctrl Pts',(-185.685591537568,-94.9071911396622,
2.9302311934868));
#29876=CARTESIAN_POINT('Ctrl Pts',(-185.601495312243,-95.0081045961674,
2.83162446606724));
#29877=CARTESIAN_POINT('Ctrl Pts',(-185.561162176427,-95.0565033932728,
2.78433199230926));
#29878=CARTESIAN_POINT('Ctrl Pts',(-185.521166286726,-95.1044349798528,
2.73613731470135));
#29879=CARTESIAN_POINT('Ctrl Pts',(-185.481581840516,-95.1518132058979,
2.68700663088748));
#29880=CARTESIAN_POINT('Ctrl Pts',(-185.459407567479,-95.1783533705557,
2.65948478072513));
#29881=CARTESIAN_POINT('Ctrl Pts',(-185.437390340001,-95.2046865189509,
2.63170922282642));
#29882=CARTESIAN_POINT('Ctrl Pts',(-185.415543190754,-95.2307980905917,
2.60366497338433));
#29883=CARTESIAN_POINT('Ctrl Pts',(-185.32184962202,-95.3427800386538,2.48339455352382));
#29884=CARTESIAN_POINT('Ctrl Pts',(-185.231198988516,-95.4507885299479,
2.35812769161362));
#29885=CARTESIAN_POINT('Ctrl Pts',(-185.14448741561,-95.5538311784959,2.22653883183237));
#29886=CARTESIAN_POINT('Ctrl Pts',(-185.118496003256,-95.5847177588987,
2.18709565024665));
#29887=CARTESIAN_POINT('Ctrl Pts',(-185.092858368683,-95.615158333568,2.14708472715111));
#29888=CARTESIAN_POINT('Ctrl Pts',(-185.067598271939,-95.6451266185791,
2.10647110827528));
#29889=CARTESIAN_POINT('Ctrl Pts',(-185.04926100973,-95.6668817332094,2.07698814207058));
#29890=CARTESIAN_POINT('Ctrl Pts',(-185.03112473284,-95.6883856466966,2.04718432923131));
#29891=CARTESIAN_POINT('Ctrl Pts',(-185.013204603834,-95.7096213333921,
2.01703659106574));
#29892=CARTESIAN_POINT('Ctrl Pts',(-184.967811845906,-95.7634125971293,
1.94067056824769));
#29893=CARTESIAN_POINT('Ctrl Pts',(-184.923807018128,-95.8154815879584,
1.86210666755521));
#29894=CARTESIAN_POINT('Ctrl Pts',(-184.881431917216,-95.8655570274556,
1.7809702719163));
#29895=CARTESIAN_POINT('Ctrl Pts',(-184.825774386239,-95.9313285599137,
1.67440175982982));
#29896=CARTESIAN_POINT('Ctrl Pts',(-184.772670985349,-95.9939632911766,
1.56273012066443));
#29897=CARTESIAN_POINT('Ctrl Pts',(-184.724064910961,-96.0512115684829,
1.4475706170276));
#29898=CARTESIAN_POINT('Ctrl Pts',(-184.720923170051,-96.0549119136995,
1.44012707569359));
#29899=CARTESIAN_POINT('Ctrl Pts',(-184.717800207441,-96.0585897677374,
1.43266895612795));
#29900=CARTESIAN_POINT('Ctrl Pts',(-184.714696543205,-96.0622445285302,
1.42519669190371));
#29901=CARTESIAN_POINT('Ctrl Pts',(-184.701735849836,-96.0775065641012,
1.39399301843432));
#29902=CARTESIAN_POINT('Ctrl Pts',(-184.689100103647,-96.0923796827891,
1.36253068298622));
#29903=CARTESIAN_POINT('Ctrl Pts',(-184.676807280731,-96.1068436897848,
1.33079541527949));
#29904=CARTESIAN_POINT('Ctrl Pts',(-184.648777871197,-96.1398237122238,
1.2584344269732));
#29905=CARTESIAN_POINT('Ctrl Pts',(-184.622509882575,-96.1707019647372,
1.18459919006109));
#29906=CARTESIAN_POINT('Ctrl Pts',(-184.598256545621,-96.199191795093,1.10925148363532));
#29907=CARTESIAN_POINT('Ctrl Pts',(-184.591076176966,-96.2076264070098,
1.08694427244499));
#29908=CARTESIAN_POINT('Ctrl Pts',(-184.584072197339,-96.215851904591,1.06450464915634));
#29909=CARTESIAN_POINT('Ctrl Pts',(-184.577250656738,-96.223861464087,1.04193203820146));
#29910=CARTESIAN_POINT('Ctrl Pts',(-184.567880266697,-96.2348637729396,
1.01092523471116));
#29911=CARTESIAN_POINT('Ctrl Pts',(-184.558842564639,-96.2454721860925,
0.979605139691351));
#29912=CARTESIAN_POINT('Ctrl Pts',(-184.550167600447,-96.2556521479711,
0.948014981072279));
#29913=CARTESIAN_POINT('Ctrl Pts',(-184.530838587854,-96.2783345022721,
0.877627765602832));
#29914=CARTESIAN_POINT('Ctrl Pts',(-184.513235022002,-96.2989782309101,
0.805566052494168));
#29915=CARTESIAN_POINT('Ctrl Pts',(-184.497723350323,-96.3171609179611,
0.732331144455422));
#29916=CARTESIAN_POINT('Ctrl Pts',(-184.490400627877,-96.3257445686055,
0.697758538997906));
#29917=CARTESIAN_POINT('Ctrl Pts',(-184.483543702019,-96.3337802274136,
0.662924800421288));
#29918=CARTESIAN_POINT('Ctrl Pts',(-184.477188558001,-96.3412264732102,
0.627883924123101));
#29919=CARTESIAN_POINT('Ctrl Pts',(-184.471708935196,-96.3476468813324,
0.597670480605272));
#29920=CARTESIAN_POINT('Ctrl Pts',(-184.466612404099,-96.3536174294331,
0.567383947479514));
#29921=CARTESIAN_POINT('Ctrl Pts',(-184.461905304076,-96.3591310153293,
0.537033589087389));
#29922=CARTESIAN_POINT('Ctrl Pts',(-184.449891188881,-96.3732035559132,
0.459569184206443));
#29923=CARTESIAN_POINT('Ctrl Pts',(-184.440391292081,-96.3843258397573,
0.381489330036032));
#29924=CARTESIAN_POINT('Ctrl Pts',(-184.433518360913,-96.3923711200197,
0.30289407795958));
#29925=CARTESIAN_POINT('Ctrl Pts',(-184.430352686432,-96.3960767788994,
0.266693077589362));
#29926=CARTESIAN_POINT('Ctrl Pts',(-184.42774387211,-96.3991301793696,0.230382778870197));
#29927=CARTESIAN_POINT('Ctrl Pts',(-184.425700498251,-96.4015217872293,
0.193973205371186));
#29928=CARTESIAN_POINT('Ctrl Pts',(-184.424156021588,-96.4033294752903,
0.166453162295789));
#29929=CARTESIAN_POINT('Ctrl Pts',(-184.422942837909,-96.4047494377422,
0.138819434141523));
#29930=CARTESIAN_POINT('Ctrl Pts',(-184.422059032266,-96.4057838996397,
0.111126891478164));
#29931=CARTESIAN_POINT('Ctrl Pts',(-184.419627274872,-96.4086301819538,
0.0349319203504133));
#29932=CARTESIAN_POINT('Ctrl Pts',(-184.41972428653,-96.4085168258584,-0.0420689086660848));
#29933=CARTESIAN_POINT('Ctrl Pts',(-184.422335964684,-96.4054599928347,
-0.1187107551091));
#29934=CARTESIAN_POINT('Ctrl Pts',(-184.423832696895,-96.4037081458698,
-0.162633594540406));
#29935=CARTESIAN_POINT('Ctrl Pts',(-184.426154715286,-96.4009902805694,
-0.206438375012906));
#29936=CARTESIAN_POINT('Ctrl Pts',(-184.429294421096,-96.3973152254108,
-0.249907542783699));
#29937=CARTESIAN_POINT('Ctrl Pts',(-184.43102093474,-96.3952943249645,-0.27381109164313));
#29938=CARTESIAN_POINT('Ctrl Pts',(-184.432987420065,-96.392992489407,-0.297635627135412));
#29939=CARTESIAN_POINT('Ctrl Pts',(-184.435188366514,-96.3904160126184,
-0.32137898897374));
#29940=CARTESIAN_POINT('Ctrl Pts',(-184.446492157098,-96.3771835443468,
-0.443321978554948));
#29941=CARTESIAN_POINT('Ctrl Pts',(-184.464046436611,-96.3566295002806,
-0.56334586016209));
#29942=CARTESIAN_POINT('Ctrl Pts',(-184.487349843213,-96.3293193460245,
-0.681667501810756));
#29943=CARTESIAN_POINT('Ctrl Pts',(-184.5093818415,-96.3034992038428,-0.793533644414358));
#29944=CARTESIAN_POINT('Ctrl Pts',(-184.53663767668,-96.2715388325085,-0.903702267157027));
#29945=CARTESIAN_POINT('Ctrl Pts',(-184.567717622243,-96.2350535477655,
-1.00994570050335));
#29946=CARTESIAN_POINT('Ctrl Pts',(-184.575817771746,-96.2255446424004,
-1.0376351857431));
#29947=CARTESIAN_POINT('Ctrl Pts',(-184.584177636599,-96.2157284231754,
-1.06505779204202));
#29948=CARTESIAN_POINT('Ctrl Pts',(-184.592772335258,-96.205633599054,-1.09217348702855));
#29949=CARTESIAN_POINT('Ctrl Pts',(-184.59770543273,-96.1998394748694,-1.10773707706353));
#29950=CARTESIAN_POINT('Ctrl Pts',(-184.602718567273,-96.1939504226047,
-1.12322340746622));
#29951=CARTESIAN_POINT('Ctrl Pts',(-184.607810241802,-96.1879681162283,
-1.13863412730332));
#29952=CARTESIAN_POINT('Ctrl Pts',(-184.668299868327,-96.1168976901068,
-1.32171509253029));
#29953=CARTESIAN_POINT('Ctrl Pts',(-184.739770298932,-96.0327883494803,
-1.49401273636365));
#29954=CARTESIAN_POINT('Ctrl Pts',(-184.819572872681,-95.9386084441054,
-1.65829837259598));
#29955=CARTESIAN_POINT('Ctrl Pts',(-184.845731358824,-95.907737212339,-1.71214956231442));
#29956=CARTESIAN_POINT('Ctrl Pts',(-184.872784849862,-95.8757841932931,
-1.76513991495109));
#29957=CARTESIAN_POINT('Ctrl Pts',(-184.90063911685,-95.8428549126627,-1.81736734120617));
#29958=CARTESIAN_POINT('Ctrl Pts',(-184.905815155924,-95.8367358055509,
-1.82707254002346));
#29959=CARTESIAN_POINT('Ctrl Pts',(-184.911017482247,-95.830584581261,-1.83674716358283));
#29960=CARTESIAN_POINT('Ctrl Pts',(-184.916245538324,-95.8244018761813,
-1.846391346213));
#29961=CARTESIAN_POINT('Ctrl Pts',(-185.010656252192,-95.7127516582894,
-2.0205505658697));
#29962=CARTESIAN_POINT('Ctrl Pts',(-185.113242298276,-95.5910902796965,
-2.18442406995139));
#29963=CARTESIAN_POINT('Ctrl Pts',(-185.220589772618,-95.4633228719102,
-2.33893888316464));
#29964=CARTESIAN_POINT('Ctrl Pts',(-185.244425496704,-95.4349530504696,
-2.37324777098454));
#29965=CARTESIAN_POINT('Ctrl Pts',(-185.268495907553,-95.4062822457651,
-2.40709506849083));
#29966=CARTESIAN_POINT('Ctrl Pts',(-185.292763461497,-95.3773533811576,
-2.44049063423734));
#29967=CARTESIAN_POINT('Ctrl Pts',(-185.297183559142,-95.3720842713572,
-2.44657330997149));
#29968=CARTESIAN_POINT('Ctrl Pts',(-185.301611885068,-95.366804592938,-2.45264320377738));
#29969=CARTESIAN_POINT('Ctrl Pts',(-185.306048293262,-95.3615145142168,
-2.45870035369677));
#29970=CARTESIAN_POINT('Ctrl Pts',(-185.39589785598,-95.2543757571472,-2.58137442868812));
#29971=CARTESIAN_POINT('Ctrl Pts',(-185.489079189921,-95.1429511391231,
-2.69884780436733));
#29972=CARTESIAN_POINT('Ctrl Pts',(-185.584265363415,-95.0287750048282,
-2.8113126906656));
#29973=CARTESIAN_POINT('Ctrl Pts',(-185.632328822657,-94.9711227242958,
-2.86810089088767));
#29974=CARTESIAN_POINT('Ctrl Pts',(-185.680902921176,-94.9127695458924,
-2.92361258261388));
#29975=CARTESIAN_POINT('Ctrl Pts',(-185.729814376138,-94.8539160603576,
-2.97787532426895));
#29976=CARTESIAN_POINT('Ctrl Pts',(-185.733340520173,-94.8496731715065,
-2.98178725538923));
#29977=CARTESIAN_POINT('Ctrl Pts',(-185.736868345131,-94.8454277768882,
-2.98569267661173));
#29978=CARTESIAN_POINT('Ctrl Pts',(-185.7403978352,-94.841179894217,-2.98959162660715));
#29979=CARTESIAN_POINT('Ctrl Pts',(-185.887261623273,-94.6644234426887,
-3.15182882080991));
#29980=CARTESIAN_POINT('Ctrl Pts',(-186.037043949676,-94.4833163076637,
-3.30292400819902));
#29981=CARTESIAN_POINT('Ctrl Pts',(-186.1887943239,-94.2989069513012,-3.44588566877327));
#29982=CARTESIAN_POINT('Ctrl Pts',(-186.191461258192,-94.2956660522995,
-3.4483981459717));
#29983=CARTESIAN_POINT('Ctrl Pts',(-186.194128789914,-94.2924241450045,
-3.45090814582523));
#29984=CARTESIAN_POINT('Ctrl Pts',(-186.196796916416,-94.2891812322754,
-3.45341567611537));
#29985=CARTESIAN_POINT('Ctrl Pts',(-186.399577749393,-94.0427159526433,
-3.64399100322999));
#29986=CARTESIAN_POINT('Ctrl Pts',(-186.605788811356,-93.7904494671224,
-3.82032278859053));
#29987=CARTESIAN_POINT('Ctrl Pts',(-186.814296226819,-93.5336032191841,
-3.98595810939003));
#29988=CARTESIAN_POINT('Ctrl Pts',(-186.922152843339,-93.4007419144332,
-4.0716378692109));
#29989=CARTESIAN_POINT('Ctrl Pts',(-187.030623659849,-93.2666554970703,
-4.15445634548737));
#29990=CARTESIAN_POINT('Ctrl Pts',(-187.139550339877,-93.1315149050411,
-4.2349092681681));
#29991=CARTESIAN_POINT('Ctrl Pts',(-187.140897687645,-93.1298433092952,
-4.23590441523151));
#29992=CARTESIAN_POINT('Ctrl Pts',(-187.142245104212,-93.1281715531462,
-4.23689920488079));
#29993=CARTESIAN_POINT('Ctrl Pts',(-187.143592589456,-93.1264996367226,
-4.23789363745222));
#29994=CARTESIAN_POINT('Ctrl Pts',(-187.464496209158,-92.7283327294232,
-4.47471776088121));
#29995=CARTESIAN_POINT('Ctrl Pts',(-187.789269587024,-92.3211070859464,
-4.69128196234316));
#29996=CARTESIAN_POINT('Ctrl Pts',(-188.11636450021,-91.9064086366411,-4.89229634560875));
#29997=CARTESIAN_POINT('Ctrl Pts',(-188.443417007439,-91.491763950584,-5.09328466852566));
#29998=CARTESIAN_POINT('Ctrl Pts',(-188.772790274538,-91.0696485747642,
-5.27872773491933));
#29999=CARTESIAN_POINT('Ctrl Pts',(-189.102923332965,-90.6416650378459,
-5.45338115469171));
#30000=CARTESIAN_POINT('Ctrl Pts',(-189.161372073137,-90.5658411666835,
-5.48418713568767));
#30001=CARTESIAN_POINT('Ctrl Pts',(-188.931799918787,-90.8638551717493,
-6.69061389410879));
#30002=CARTESIAN_POINT('Ctrl Pts',(-189.319051118431,-91.5508432961055,
-7.67806776636097));
#30003=CARTESIAN_POINT('Ctrl Pts',(-188.480882259406,-91.4492167738639,
-5.12686171816464));
#30004=CARTESIAN_POINT('Ctrl Pts',(-188.247114981151,-91.7480740803052,
-6.24241270393816));
#30005=CARTESIAN_POINT('Ctrl Pts',(-188.54325607873,-92.4017170418249,-7.17763983002507));
#30006=CARTESIAN_POINT('Ctrl Pts',(-187.802447662738,-92.3090870122729,
-4.72452254737714));
#30007=CARTESIAN_POINT('Ctrl Pts',(-187.560117152723,-92.6143626232248,
-5.74091658805703));
#30008=CARTESIAN_POINT('Ctrl Pts',(-187.770816940042,-93.2269599088197,
-6.61450397286226));
#30009=CARTESIAN_POINT('Ctrl Pts',(-186.817594622089,-93.5309513688875,
-3.99710358618598));
#30010=CARTESIAN_POINT('Ctrl Pts',(-186.560018651586,-93.8482869695348,
-4.84090069541392));
#30011=CARTESIAN_POINT('Ctrl Pts',(-186.649906375822,-94.3967003926096,
-5.59609535962116));
#30012=CARTESIAN_POINT('Ctrl Pts',(-186.49935620113,-93.9215074314833,-3.73845962749932));
#30013=CARTESIAN_POINT('Ctrl Pts',(-186.237740008661,-94.2416057943953,
-4.52342407349232));
#30014=CARTESIAN_POINT('Ctrl Pts',(-186.287822634423,-94.7700540089429,
-5.2339853240387));
#30015=CARTESIAN_POINT('Ctrl Pts',(-186.033516383533,-94.4876030676821,
-3.29959059467639));
#30016=CARTESIAN_POINT('Ctrl Pts',(-185.765439319798,-94.812289584031,-3.98645759369846));
#30017=CARTESIAN_POINT('Ctrl Pts',(-185.757965731837,-95.3104885264767,
-4.61955372496917));
#30018=CARTESIAN_POINT('Ctrl Pts',(-185.88019021819,-94.6729739327449,-3.14470232538271));
#30019=CARTESIAN_POINT('Ctrl Pts',(-185.610178683132,-94.9989268771276,
-3.79762392135999));
#30020=CARTESIAN_POINT('Ctrl Pts',(-185.58359686481,-95.487331712576,-4.40270469240992));
#30021=CARTESIAN_POINT('Ctrl Pts',(-185.579441491387,-95.0348546295449,
-2.81104162230377));
#30022=CARTESIAN_POINT('Ctrl Pts',(-185.305657248066,-95.3632353428488,
-3.39170158162171));
#30023=CARTESIAN_POINT('Ctrl Pts',(-185.241624386475,-95.8323366660802,
-3.9355677050804));
#30024=CARTESIAN_POINT('Ctrl Pts',(-185.432149758444,-95.2111937660602,
-2.63230461390661));
#30025=CARTESIAN_POINT('Ctrl Pts',(-185.156486831618,-95.5407893224819,
-3.17469909151543));
#30026=CARTESIAN_POINT('Ctrl Pts',(-185.074169959165,-96.0003339135652,
-3.68532933447742));
#30027=CARTESIAN_POINT('Ctrl Pts',(-185.153379734502,-95.5435099326639,
-2.24867201143562));
#30028=CARTESIAN_POINT('Ctrl Pts',(-184.874210151461,-95.8753214389257,
-2.70985007643056));
#30029=CARTESIAN_POINT('Ctrl Pts',(-184.757282758836,-96.3167375829767,
-3.14822934533189));
#30030=CARTESIAN_POINT('Ctrl Pts',(-185.020222521866,-95.7014835433405,
-2.04158414607404));
#30031=CARTESIAN_POINT('Ctrl Pts',(-184.73933109304,-96.0343990644554,-2.45936299143546));
#30032=CARTESIAN_POINT('Ctrl Pts',(-184.60594168315,-96.467044303765,-2.85829845866346));
#30033=CARTESIAN_POINT('Ctrl Pts',(-184.781064427074,-95.9842159788078,
-1.5931390922202));
#30034=CARTESIAN_POINT('Ctrl Pts',(-184.497157491449,-96.3190061700533,
-1.91787402398805));
#30035=CARTESIAN_POINT('Ctrl Pts',(-184.334155197262,-96.7359192863337,
-2.23045805383467));
#30036=CARTESIAN_POINT('Ctrl Pts',(-184.67579092861,-96.1081248174892,-1.3540404464544));
#30037=CARTESIAN_POINT('Ctrl Pts',(-184.390491452695,-96.443809197977,-1.62954253866593));
#30038=CARTESIAN_POINT('Ctrl Pts',(-184.214536143277,-96.853680548758,-1.89571059383307));
#30039=CARTESIAN_POINT('Ctrl Pts',(-184.551305176205,-96.2543384967701,
-0.961207376325233));
#30040=CARTESIAN_POINT('Ctrl Pts',(-184.264389274944,-96.5910392742284,
-1.1563047628428));
#30041=CARTESIAN_POINT('Ctrl Pts',(-184.073096480939,-96.9925975894506,
-1.34572877555771));
#30042=CARTESIAN_POINT('Ctrl Pts',(-184.515191334187,-96.2966908244908,
-0.822876876373191));
#30043=CARTESIAN_POINT('Ctrl Pts',(-184.227811011248,-96.6336802570244,
-0.989790943527011));
#30044=CARTESIAN_POINT('Ctrl Pts',(-184.032066276688,-97.0328274290813,
-1.15206057370444));
#30045=CARTESIAN_POINT('Ctrl Pts',(-184.459543757323,-96.3619063746552,
-0.540441124341592));
#30046=CARTESIAN_POINT('Ctrl Pts',(-184.17146012754,-96.6993255241945,-0.649971919835621));
#30047=CARTESIAN_POINT('Ctrl Pts',(-183.968844518678,-97.094768498995,-0.756639241730944));
#30048=CARTESIAN_POINT('Ctrl Pts',(-184.439877210306,-96.384927969357,-0.3966207303986));
#30049=CARTESIAN_POINT('Ctrl Pts',(-184.151539311701,-96.7225052514127,
-0.476968102648842));
#30050=CARTESIAN_POINT('Ctrl Pts',(-183.94650199697,-97.1166305263899,-0.555284933855703));
#30051=CARTESIAN_POINT('Ctrl Pts',(-184.418726617447,-96.4096849406706,
-0.103191726055235));
#30052=CARTESIAN_POINT('Ctrl Pts',(-184.13012131677,-96.7474252069729,-0.124096554342044));
#30053=CARTESIAN_POINT('Ctrl Pts',(-183.922473553532,-97.1401402657989,
-0.144472556946369));
#30054=CARTESIAN_POINT('Ctrl Pts',(-184.417514594902,-96.4111027446528,
0.0472614384591417));
#30055=CARTESIAN_POINT('Ctrl Pts',(-184.128893590219,-96.7488527806606,
0.0568388822194814));
#30056=CARTESIAN_POINT('Ctrl Pts',(-183.921096645597,-97.1414865203694,
0.0661679095530208));
#30057=CARTESIAN_POINT('Ctrl Pts',(-184.433928343805,-96.3918917393423,
0.340679262061748));
#30058=CARTESIAN_POINT('Ctrl Pts',(-184.145514858577,-96.7295153091363,
0.409686266430749));
#30059=CARTESIAN_POINT('Ctrl Pts',(-183.939743681783,-97.1232435467616,
0.476964636235577));
#30060=CARTESIAN_POINT('Ctrl Pts',(-184.451318549818,-96.3715380527475,
0.485263899435256));
#30061=CARTESIAN_POINT('Ctrl Pts',(-184.163130050764,-96.7090216702262,
0.58359947105962));
#30062=CARTESIAN_POINT('Ctrl Pts',(-183.959500024897,-97.1039154961823,
0.679388918539565));
#30063=CARTESIAN_POINT('Ctrl Pts',(-184.503065282061,-96.3109070247479,
0.770500979869548));
#30064=CARTESIAN_POINT('Ctrl Pts',(-184.215530826723,-96.6479911950592,
0.926759235444962));
#30065=CARTESIAN_POINT('Ctrl Pts',(-184.018289586001,-97.0463305526287,
1.07873223115544));
#30066=CARTESIAN_POINT('Ctrl Pts',(-184.537197371241,-96.2708903134169,
0.909351028970219));
#30067=CARTESIAN_POINT('Ctrl Pts',(-184.250102220423,-96.6077014142732,
1.09388043094421));
#30068=CARTESIAN_POINT('Ctrl Pts',(-184.057067888501,-97.0083208724158,
1.27312782793969));
#30069=CARTESIAN_POINT('Ctrl Pts',(-184.617313485274,-96.1768214097042,
1.17450600394552));
#30070=CARTESIAN_POINT('Ctrl Pts',(-184.331230366073,-96.5130118325845,
1.41315289922425));
#30071=CARTESIAN_POINT('Ctrl Pts',(-184.148094181734,-96.9189506155886,
1.64435530785332));
#30072=CARTESIAN_POINT('Ctrl Pts',(-184.663509817147,-96.1225201391488,
1.30195095812244));
#30073=CARTESIAN_POINT('Ctrl Pts',(-184.378018762994,-96.4583417814738,
1.56670202993));
#30074=CARTESIAN_POINT('Ctrl Pts',(-184.200583375354,-96.8673534301572,
1.82278327080832));
#30075=CARTESIAN_POINT('Ctrl Pts',(-184.765892134559,-96.0019584784386,
1.54843340014367));
#30076=CARTESIAN_POINT('Ctrl Pts',(-184.481693345806,-96.3369830067698,
1.86384266651038));
#30077=CARTESIAN_POINT('Ctrl Pts',(-184.316918986678,-96.7527656506066,
2.16786835852121));
#30078=CARTESIAN_POINT('Ctrl Pts',(-184.822258965331,-95.9354828021284,
1.66765797593972));
#30079=CARTESIAN_POINT('Ctrl Pts',(-184.538778909602,-96.2700583618635,
2.00767566272329));
#30080=CARTESIAN_POINT('Ctrl Pts',(-184.38097095927,-96.689570118882,2.33478741094054));
#30081=CARTESIAN_POINT('Ctrl Pts',(-184.940610822495,-95.7956242175333,
1.89427491600705));
#30082=CARTESIAN_POINT('Ctrl Pts',(-184.658623126078,-96.1292728064777,
2.28126505316723));
#30083=CARTESIAN_POINT('Ctrl Pts',(-184.515467826532,-96.5565741281235,
2.65205989789117));
#30084=CARTESIAN_POINT('Ctrl Pts',(-185.002889262547,-95.7218966402254,
2.00242188310173));
#30085=CARTESIAN_POINT('Ctrl Pts',(-184.721692402306,-96.0550488275035,
2.41193520152812));
#30086=CARTESIAN_POINT('Ctrl Pts',(-184.58624608764,-96.4864461947272,2.80346980635789));
#30087=CARTESIAN_POINT('Ctrl Pts',(-185.197026331985,-95.4915746624195,
2.31455411749728));
#30088=CARTESIAN_POINT('Ctrl Pts',(-184.918382736524,-95.8230687547819,
2.78959213143254));
#30089=CARTESIAN_POINT('Ctrl Pts',(-184.806894376427,-96.2673020072735,
3.24046678270688));
#30090=CARTESIAN_POINT('Ctrl Pts',(-185.336085584367,-95.3259562568104,
2.50639205883812));
#30091=CARTESIAN_POINT('Ctrl Pts',(-185.05923035822,-95.6562990966472,3.02200207733063));
#30092=CARTESIAN_POINT('Ctrl Pts',(-184.964963155496,-96.1096343126113,
3.50904708677375));
#30093=CARTESIAN_POINT('Ctrl Pts',(-185.627101504566,-94.9776421379489,
2.8675740869709));
#30094=CARTESIAN_POINT('Ctrl Pts',(-185.353902675123,-95.3056561818072,
3.46039964178234));
#30095=CARTESIAN_POINT('Ctrl Pts',(-185.295813082335,-95.7778102261891,
4.01471521208864));
#30096=CARTESIAN_POINT('Ctrl Pts',(-185.777854592945,-94.7963843918386,
3.03519751521752));
#30097=CARTESIAN_POINT('Ctrl Pts',(-185.506567110887,-95.1231570680354,
3.66427460436627));
#30098=CARTESIAN_POINT('Ctrl Pts',(-185.467225951133,-95.6050234038876,
4.24939405589426));
#30099=CARTESIAN_POINT('Ctrl Pts',(-186.236474409762,-94.2421557863911,
3.50623173805454));
#30100=CARTESIAN_POINT('Ctrl Pts',(-185.971545136454,-94.5644641073805,
4.2391615355178));
#30101=CARTESIAN_POINT('Ctrl Pts',(-185.988779734173,-95.0763236040051,
4.90885842617087));
#30102=CARTESIAN_POINT('Ctrl Pts',(-186.552577188049,-93.8564712961017,
3.78096556310273));
#30103=CARTESIAN_POINT('Ctrl Pts',(-186.291689470114,-94.1760351311294,
4.57551417638629));
#30104=CARTESIAN_POINT('Ctrl Pts',(-186.348368737014,-94.7079178118668,
5.29349504960836));
#30105=CARTESIAN_POINT('Ctrl Pts',(-187.194773811378,-93.0643566503644,
4.28435082011719));
#30106=CARTESIAN_POINT('Ctrl Pts',(-186.941883309471,-93.3785228823314,
5.19477666592858));
#30107=CARTESIAN_POINT('Ctrl Pts',(-187.079154956339,-93.950182287929,5.99825056968396));
#30108=CARTESIAN_POINT('Ctrl Pts',(-187.521076674221,-92.6576892683202,
4.51235264699091));
#30109=CARTESIAN_POINT('Ctrl Pts',(-187.272289578896,-92.9689762843847,
5.47665603794965));
#30110=CARTESIAN_POINT('Ctrl Pts',(-187.450589338641,-93.5606283707695,
6.31746005549287));
#30111=CARTESIAN_POINT('Ctrl Pts',(-188.179111216884,-91.8283620827728,
4.93577418367053));
#30112=CARTESIAN_POINT('Ctrl Pts',(-187.938458966174,-92.1339334046923,
6.0029378771628));
#30113=CARTESIAN_POINT('Ctrl Pts',(-188.199887644392,-92.7650449264735,
6.91026231965974));
#30114=CARTESIAN_POINT('Ctrl Pts',(-188.511250209779,-91.4051637127826,
5.13113846602503));
#30115=CARTESIAN_POINT('Ctrl Pts',(-188.274704695279,-91.7077535346966,
6.24708719969882));
#30116=CARTESIAN_POINT('Ctrl Pts',(-188.578215964155,-92.3584957265317,
7.18377754322972));
#30117=CARTESIAN_POINT('Ctrl Pts',(-189.172005963988,-90.553639486457,5.49397424413352));
#30118=CARTESIAN_POINT('Ctrl Pts',(-188.943562752701,-90.8502999646729,
6.70318459853149));
#30119=CARTESIAN_POINT('Ctrl Pts',(-189.331108638081,-91.5393071732205,
7.69175665054725));
#30120=CARTESIAN_POINT('Ctrl Pts',(-189.501522189065,-90.1241962177521,
5.66196658596113));
#30121=CARTESIAN_POINT('Ctrl Pts',(-189.277097989269,-90.4178279861717,
6.91560519707551));
#30122=CARTESIAN_POINT('Ctrl Pts',(-189.706696752647,-91.1255979019193,
7.92694977629545));
#30123=CARTESIAN_POINT('Ctrl Pts',(-190.486239445227,-88.8261079680731,
6.13501898383449));
#30124=CARTESIAN_POINT('Ctrl Pts',(-190.276817167461,-89.1066399409558,
7.51936598512612));
#30125=CARTESIAN_POINT('Ctrl Pts',(-190.829455494059,-89.8733451950527,
8.58923262591312));
#30126=CARTESIAN_POINT('Ctrl Pts',(-191.137549166309,-87.9477683977818,
6.40961295141922));
#30127=CARTESIAN_POINT('Ctrl Pts',(-190.935907302917,-88.2219096053228,
7.87329503257363));
#30128=CARTESIAN_POINT('Ctrl Pts',(-191.572553975477,-89.0237350610749,
8.9736687655578));
#30129=CARTESIAN_POINT('Ctrl Pts',(-192.426096187629,-86.1688927511435,
6.90461427891117));
#30130=CARTESIAN_POINT('Ctrl Pts',(-192.239840939106,-86.4303069194794,
8.52054279716209));
#30131=CARTESIAN_POINT('Ctrl Pts',(-193.043608084131,-87.2985121886298,
9.66667669899339));
#30132=CARTESIAN_POINT('Ctrl Pts',(-193.063383291067,-85.2683028918415,
7.12463735631982));
#30133=CARTESIAN_POINT('Ctrl Pts',(-192.884538179013,-85.5231335814101,
8.81258405161933));
#30134=CARTESIAN_POINT('Ctrl Pts',(-193.771620169991,-86.422849070216,9.97471067331157));
#30135=CARTESIAN_POINT('Ctrl Pts',(-194.951173747053,-82.5359543744168,
7.72418030763633));
#30136=CARTESIAN_POINT('Ctrl Pts',(-194.806418839045,-82.7536742244153,
9.62675633492785));
#30137=CARTESIAN_POINT('Ctrl Pts',(-195.929442725192,-83.7595332915572,
10.8140713899068));
#30138=CARTESIAN_POINT('Ctrl Pts',(-196.177482368031,-80.6737566961289,
8.04415647989996));
#30139=CARTESIAN_POINT('Ctrl Pts',(-196.045620897114,-80.8772001990853,
10.0746117618081));
#30140=CARTESIAN_POINT('Ctrl Pts',(-197.332903494677,-81.9356779296839,
11.2620353059768));
#30141=CARTESIAN_POINT('Ctrl Pts',(-197.961738112988,-77.8250108254079,
8.44922123457211));
#30142=CARTESIAN_POINT('Ctrl Pts',(-197.838189296233,-78.0258804597084,
10.662721491043));
#30143=CARTESIAN_POINT('Ctrl Pts',(-199.377119697722,-79.1331363472436,
11.8291181367819));
#30144=CARTESIAN_POINT('Ctrl Pts',(-198.54807446978,-76.8648659123181,8.57151350105634));
#30145=CARTESIAN_POINT('Ctrl Pts',(-198.430673215286,-77.058817715059,10.8457736874515));
#30146=CARTESIAN_POINT('Ctrl Pts',(-200.049262590727,-78.1865264035749,
12.0003238810597));
#30147=CARTESIAN_POINT('Ctrl Pts',(-199.69669086874,-74.9349603932302,8.79383680879332));
#30148=CARTESIAN_POINT('Ctrl Pts',(-199.591479554328,-75.1150846943871,
11.1873231733843));
#30149=CARTESIAN_POINT('Ctrl Pts',(-201.366657824558,-76.2799025943682,
12.3115686050633));
#30150=CARTESIAN_POINT('Ctrl Pts',(-200.259254660993,-73.9648229368186,
8.89394683892728));
#30151=CARTESIAN_POINT('Ctrl Pts',(-200.15966038367,-74.1381129626944,11.3455724974083));
#30152=CARTESIAN_POINT('Ctrl Pts',(-202.012234149144,-75.3195244447861,
12.4517182455822));
#30153=CARTESIAN_POINT('Ctrl Pts',(-201.911900353393,-71.0391139491143,
9.16677201385288));
#30154=CARTESIAN_POINT('Ctrl Pts',(-201.839869083933,-71.1727960227069,
11.7929874150389));
#30155=CARTESIAN_POINT('Ctrl Pts',(-203.909676512503,-72.417697848325,12.8336586580376));
#30156=CARTESIAN_POINT('Ctrl Pts',(-202.966948680821,-69.0682588598496,
9.31223534270219));
#30157=CARTESIAN_POINT('Ctrl Pts',(-202.903401297136,-69.1888071156211,
12.0477177288761));
#30158=CARTESIAN_POINT('Ctrl Pts',(-205.122271910769,-70.4555661236282,
13.0372964661862));
#30159=CARTESIAN_POINT('Ctrl Pts',(-204.984382623087,-65.0867669085141,
9.55122215802441));
#30160=CARTESIAN_POINT('Ctrl Pts',(-204.939612388158,-65.1801116420663,
12.5011483784476));
#30161=CARTESIAN_POINT('Ctrl Pts',(-207.442952278212,-66.4783823872744,
13.3718543161712));
#30162=CARTESIAN_POINT('Ctrl Pts',(-205.946770795552,-63.0761264005556,
9.64459843557726));
#30163=CARTESIAN_POINT('Ctrl Pts',(-205.908524096743,-63.1571838509651,
12.6978518194603));
#30164=CARTESIAN_POINT('Ctrl Pts',(-208.55104128046,-64.4633260703388,13.5025686131142));
#30165=CARTESIAN_POINT('Ctrl Pts',(-208.695489133502,-56.9854174908883,
9.86749344216803));
#30166=CARTESIAN_POINT('Ctrl Pts',(-208.714440707254,-56.9510842463801,
13.2317085155052));
#30167=CARTESIAN_POINT('Ctrl Pts',(-211.718302688857,-58.3414499489575,
13.8145821321649));
#30168=CARTESIAN_POINT('Ctrl Pts',(-210.343625285675,-52.8466938714345,
9.94066884241106));
#30169=CARTESIAN_POINT('Ctrl Pts',(-210.359356788339,-52.7988261518928,
13.4932979556555));
#30170=CARTESIAN_POINT('Ctrl Pts',(-213.6207465057,-54.1580470864287,13.9170012070984));
#30171=CARTESIAN_POINT('Ctrl Pts',(-213.268421736275,-44.4139346324368,
10.0094381670324));
#30172=CARTESIAN_POINT('Ctrl Pts',(-213.300660782719,-44.3236097006244,
13.9242034321311));
#30173=CARTESIAN_POINT('Ctrl Pts',(-217.000471678509,-45.5970270857608,
14.0132264874685));
#30174=CARTESIAN_POINT('Ctrl Pts',(-214.545123000096,-40.1198955494031,
10.0043954519788));
#30175=CARTESIAN_POINT('Ctrl Pts',(-214.567879102413,-40.0304829990944,
14.0859702100237));
#30176=CARTESIAN_POINT('Ctrl Pts',(-218.477811583319,-41.2193854803596,
14.006142250762));
#30177=CARTESIAN_POINT('Ctrl Pts',(-215.901813979384,-34.6533359908493,
9.97920576186224));
#30178=CARTESIAN_POINT('Ctrl Pts',(-215.908024394789,-34.6277287515398,
14.2483264968055));
#30179=CARTESIAN_POINT('Ctrl Pts',(-220.048870888242,-35.6292883846372,
13.9708493230874));
#30180=CARTESIAN_POINT('Ctrl Pts',(-216.161175736962,-33.5548628771818,
9.97318130845029));
#30181=CARTESIAN_POINT('Ctrl Pts',(-216.167513463505,-33.5274498556477,
14.2791323437868));
#30182=CARTESIAN_POINT('Ctrl Pts',(-220.349283740659,-34.5051513167286,
13.9624098056824));
#30183=CARTESIAN_POINT('Ctrl Pts',(-216.653433306906,-31.3585593368,9.95985565386096));
#30184=CARTESIAN_POINT('Ctrl Pts',(-216.660220044528,-31.3274073221036,
14.3367297864681));
#30185=CARTESIAN_POINT('Ctrl Pts',(-220.919563852235,-32.2560153447119,
13.9437437591944));
#30186=CARTESIAN_POINT('Ctrl Pts',(-216.886667558864,-30.2594147169127,
9.95254907226771));
#30187=CARTESIAN_POINT('Ctrl Pts',(-216.893354457392,-30.2271777338965,
14.3635046211515));
#30188=CARTESIAN_POINT('Ctrl Pts',(-221.189823038788,-31.1296731902609,
13.9335096921047));
#30189=CARTESIAN_POINT('Ctrl Pts',(-217.548036348995,-26.959026649267,9.92956539342116));
#30190=CARTESIAN_POINT('Ctrl Pts',(-217.557469895028,-26.9096587272592,
14.4387837536445));
#30191=CARTESIAN_POINT('Ctrl Pts',(-221.956310708416,-27.7455981308832,
13.9013186781023));
#30192=CARTESIAN_POINT('Ctrl Pts',(-217.93785725504,-24.7548304673619,9.91285560896132));
#30193=CARTESIAN_POINT('Ctrl Pts',(-217.945529771334,-24.7081239842741,
14.4813778884191));
#30194=CARTESIAN_POINT('Ctrl Pts',(-222.408272062777,-25.4828152750478,
13.8779166271282));
#30195=CARTESIAN_POINT('Ctrl Pts',(-218.956084319915,-18.1305693881788,
9.86431151402464));
#30196=CARTESIAN_POINT('Ctrl Pts',(-218.968961981201,-18.0402471088626,
14.5919583080073));
#30197=CARTESIAN_POINT('Ctrl Pts',(-223.589086522611,-18.6763260278863,
13.8099328970237));
#30198=CARTESIAN_POINT('Ctrl Pts',(-219.43355866175,-13.6988539781417,9.83453026559723));
#30199=CARTESIAN_POINT('Ctrl Pts',(-219.437341306434,-13.6472841751431,
14.6400615162957));
#30200=CARTESIAN_POINT('Ctrl Pts',(-224.143198140478,-14.1144924088059,
13.7682283895981));
#30201=CARTESIAN_POINT('Ctrl Pts',(-219.989119888241,-4.80453737519254,
9.79912404538294));
#30202=CARTESIAN_POINT('Ctrl Pts',(-219.990808009853,-4.76842009685111,
14.6969168202861));
#30203=CARTESIAN_POINT('Ctrl Pts',(-224.787967419755,-4.95238819466783,
13.7186471999943));
#30204=CARTESIAN_POINT('Ctrl Pts',(-220.067212631373,-0.341936575327023,
9.79351850253299));
#30205=CARTESIAN_POINT('Ctrl Pts',(-220.067252895393,-0.352942294886242,
14.7045953323717));
#30206=CARTESIAN_POINT('Ctrl Pts',(-224.878634407894,-0.352086946103674,
13.7107976404735));
#30207=CARTESIAN_POINT('Ctrl Pts',(-219.879909693335,6.3755153565872,9.80594542214121));
#30208=CARTESIAN_POINT('Ctrl Pts',(-219.880497380835,6.35920093150428,14.6855459823587));
#30209=CARTESIAN_POINT('Ctrl Pts',(-224.661228872703,6.57039409955349,13.7281995569326));
#30210=CARTESIAN_POINT('Ctrl Pts',(-219.766658024021,8.6185966931961,9.81343805283997));
#30211=CARTESIAN_POINT('Ctrl Pts',(-219.768189961766,8.59324909174053,14.674087697868));
#30212=CARTESIAN_POINT('Ctrl Pts',(-224.529776865697,8.88156586473323,13.7386918030301));
#30213=CARTESIAN_POINT('Ctrl Pts',(-219.519208793803,11.989216125175,9.82890166451564));
#30214=CARTESIAN_POINT('Ctrl Pts',(-219.521220785067,11.9640388382862,14.6486293437786));
#30215=CARTESIAN_POINT('Ctrl Pts',(-224.242610932278,12.3530020325013,13.7603463988469));
#30216=CARTESIAN_POINT('Ctrl Pts',(-219.423742238738,13.1138355507161,9.83475451804771));
#30217=CARTESIAN_POINT('Ctrl Pts',(-219.426178170639,13.0864560589663,14.6387997480619));
#30218=CARTESIAN_POINT('Ctrl Pts',(-224.131827752852,13.5110087439763,13.7685425281566));
#30219=CARTESIAN_POINT('Ctrl Pts',(-219.207901176056,15.3538587218567,9.84754794128088));
#30220=CARTESIAN_POINT('Ctrl Pts',(-219.211013282027,15.3236509834499,14.6164107984345));
#30221=CARTESIAN_POINT('Ctrl Pts',(-223.881381580398,15.8168790115975,13.7864581223482));
#30222=CARTESIAN_POINT('Ctrl Pts',(-219.087434557838,16.4706719074987,9.85449428714415));
#30223=CARTESIAN_POINT('Ctrl Pts',(-219.091012905236,16.438758408704,14.6038650095587));
#30224=CARTESIAN_POINT('Ctrl Pts',(-223.741611655969,16.9661945554948,13.7961856778895));
#30225=CARTESIAN_POINT('Ctrl Pts',(-218.422980077555,22.0388998567845,9.89118647406901));
#30226=CARTESIAN_POINT('Ctrl Pts',(-218.433419066376,21.9590251220096,14.5345785986599));
#30227=CARTESIAN_POINT('Ctrl Pts',(-222.97077617523,22.6944728454244,13.8475694404199));
#30228=CARTESIAN_POINT('Ctrl Pts',(-217.693018709706,26.4429011459421,9.92732876816581));
#30229=CARTESIAN_POINT('Ctrl Pts',(-217.714959019159,26.3354267756488,14.4579318865959));
#30230=CARTESIAN_POINT('Ctrl Pts',(-222.124173803383,27.2186160038052,13.8981845777223));
#30231=CARTESIAN_POINT('Ctrl Pts',(-215.845448226668,35.1520276824801,9.98467680865933));
#30232=CARTESIAN_POINT('Ctrl Pts',(-215.866013311531,35.0590051000879,14.2452448518599));
#30233=CARTESIAN_POINT('Ctrl Pts',(-219.983341103331,36.1431189089753,13.97851024857));
#30234=CARTESIAN_POINT('Ctrl Pts',(-214.727821174011,39.4571485295923,10.0059888635688));
#30235=CARTESIAN_POINT('Ctrl Pts',(-214.759629081728,39.3546193987856,14.1128925867739));
#30236=CARTESIAN_POINT('Ctrl Pts',(-218.689081945027,40.54350160402,14.0083695379852));
#30237=CARTESIAN_POINT('Ctrl Pts',(-212.104461778024,47.9683278252243,9.99106655001064));
#30238=CARTESIAN_POINT('Ctrl Pts',(-212.124917932219,47.9013202094227,13.7573388162155));
#30239=CARTESIAN_POINT('Ctrl Pts',(-215.654940347415,49.2109673894579,13.9875274814399));
#30240=CARTESIAN_POINT('Ctrl Pts',(-210.598749993438,52.1743923065104,9.95531537581287));
#30241=CARTESIAN_POINT('Ctrl Pts',(-210.626152534245,52.1133929267026,13.5405466970593));
#30242=CARTESIAN_POINT('Ctrl Pts',(-213.915067425145,53.4780843735008,13.9375020387498));
#30243=CARTESIAN_POINT('Ctrl Pts',(-208.467801042867,57.3684010647384,9.83445365866558));
#30244=CARTESIAN_POINT('Ctrl Pts',(-208.440496676423,57.4335485585645,13.1675008632595));
#30245=CARTESIAN_POINT('Ctrl Pts',(-211.45675431658,58.7206047789808,13.7683295199504));
#30246=CARTESIAN_POINT('Ctrl Pts',(-208.029146170907,58.4040178152079,9.80639282881666));
#30247=CARTESIAN_POINT('Ctrl Pts',(-207.998880661217,58.4750011351285,13.0896849260068));
#30248=CARTESIAN_POINT('Ctrl Pts',(-210.950890758971,59.7645343781391,13.7290510241888));
#30249=CARTESIAN_POINT('Ctrl Pts',(-207.12664788482,60.4688131192695,9.74108338571404));
#30250=CARTESIAN_POINT('Ctrl Pts',(-207.089446964967,60.5522052555366,12.9231741124707));
#30251=CARTESIAN_POINT('Ctrl Pts',(-209.910535831253,61.8429955994894,13.6376310670489));
#30252=CARTESIAN_POINT('Ctrl Pts',(-206.662970155658,61.4975272274392,9.70383665509011));
#30253=CARTESIAN_POINT('Ctrl Pts',(-206.62229251033,61.587147971588,12.8346671765189));
#30254=CARTESIAN_POINT('Ctrl Pts',(-209.376236001022,62.8770556591804,13.5854922099582));
#30255=CARTESIAN_POINT('Ctrl Pts',(-205.240266007795,64.5604067343896,9.5765196532658));
#30256=CARTESIAN_POINT('Ctrl Pts',(-205.196584633148,64.650427049727,12.5533538086537));
#30257=CARTESIAN_POINT('Ctrl Pts',(-207.737539989063,65.9512466063413,13.4072675873146));
#30258=CARTESIAN_POINT('Ctrl Pts',(-204.247673314577,66.5757395952135,9.47090861845935));
#30259=CARTESIAN_POINT('Ctrl Pts',(-204.196792574619,66.6787164938637,12.3422625706762));
#30260=CARTESIAN_POINT('Ctrl Pts',(-206.595163150902,67.9678447656868,13.259424414464));
#30261=CARTESIAN_POINT('Ctrl Pts',(-202.175877209204,70.5527743625175,9.20351075943804));
#30262=CARTESIAN_POINT('Ctrl Pts',(-202.105162467068,70.6833454593898,11.8563179607818));
#30263=CARTESIAN_POINT('Ctrl Pts',(-204.213034709984,71.9338913959523,12.8850903188223));
#30264=CARTESIAN_POINT('Ctrl Pts',(-201.096663082113,72.5144855502291,9.04188771001516));
#30265=CARTESIAN_POINT('Ctrl Pts',(-201.016769126083,72.6586875911064,11.5835583962009));
#30266=CARTESIAN_POINT('Ctrl Pts',(-202.973270051406,73.8833489271374,12.6588283062611));
#30267=CARTESIAN_POINT('Ctrl Pts',(-198.853190944606,76.3831310032251,8.64078280219066));
#30268=CARTESIAN_POINT('Ctrl Pts',(-198.749688199617,76.5553396176626,10.9496183488417));
#30269=CARTESIAN_POINT('Ctrl Pts',(-200.398794120576,77.7129932538224,12.097299012796));
#30270=CARTESIAN_POINT('Ctrl Pts',(-197.688906293114,78.2900912932045,8.4017397701364));
#30271=CARTESIAN_POINT('Ctrl Pts',(-197.574275171399,78.4761661484505,10.5915528796197));
#30272=CARTESIAN_POINT('Ctrl Pts',(-199.064051750511,79.593204560045,11.7626455547735));
#30273=CARTESIAN_POINT('Ctrl Pts',(-195.880204369929,81.1077158340626,7.95715194188713));
#30274=CARTESIAN_POINT('Ctrl Pts',(-195.7336336546,81.3323663938434,9.95197272056883));
#30275=CARTESIAN_POINT('Ctrl Pts',(-196.992976264055,82.3591154501006,11.1402297609643));
#30276=CARTESIAN_POINT('Ctrl Pts',(-195.266929615523,82.0397774649153,7.79447520511931));
#30277=CARTESIAN_POINT('Ctrl Pts',(-195.113586791239,82.271187103462,9.7241882232041));
#30278=CARTESIAN_POINT('Ctrl Pts',(-196.291129043696,83.2720093140021,10.9124837103213));
#30279=CARTESIAN_POINT('Ctrl Pts',(-194.020039407559,83.8890943957255,7.43221244761711));
#30280=CARTESIAN_POINT('Ctrl Pts',(-193.852340906558,84.1338848996827,9.22650488428313));
#30281=CARTESIAN_POINT('Ctrl Pts',(-194.865016774257,85.0790184789678,10.4053168524648));
#30282=CARTESIAN_POINT('Ctrl Pts',(-193.386270744956,84.8064721381628,7.2325858360569));
#30283=CARTESIAN_POINT('Ctrl Pts',(-193.211305013333,85.0579843658949,8.9571159136994));
#30284=CARTESIAN_POINT('Ctrl Pts',(-194.140578625951,85.9732430528797,10.1258390890344));
#30285=CARTESIAN_POINT('Ctrl Pts',(-192.107819334031,86.61357210353,6.78753527125637));
#30286=CARTESIAN_POINT('Ctrl Pts',(-191.917758060802,86.8780799988377,8.36623872478481));
#30287=CARTESIAN_POINT('Ctrl Pts',(-192.680140055584,87.7303403765514,9.50276493243055));
#30288=CARTESIAN_POINT('Ctrl Pts',(-191.462180488014,87.5047202513877,6.54205946399846));
#30289=CARTESIAN_POINT('Ctrl Pts',(-191.264472823669,87.7757783231601,8.04532402545658));
#30290=CARTESIAN_POINT('Ctrl Pts',(-191.943046059177,88.5946069753687,9.15909579322666));
#30291=CARTESIAN_POINT('Ctrl Pts',(-190.150638039327,89.2738373630881,5.98189948503679));
#30292=CARTESIAN_POINT('Ctrl Pts',(-189.937244247952,89.5572864784185,7.32319343760467));
#30293=CARTESIAN_POINT('Ctrl Pts',(-190.446683438805,90.3058737452788,8.37486245635653));
#30294=CARTESIAN_POINT('Ctrl Pts',(-189.484435938415,90.1514762972045,5.66676146619764));
#30295=CARTESIAN_POINT('Ctrl Pts',(-189.262882995061,90.4414214467756,6.92234530392305));
#30296=CARTESIAN_POINT('Ctrl Pts',(-189.687009990413,91.1525614199763,7.93360765281502));
#30297=CARTESIAN_POINT('Ctrl Pts',(-188.817225428583,91.010840855218,5.29913391686224));
#30298=CARTESIAN_POINT('Ctrl Pts',(-188.583433673891,91.3119644595324,6.4575852679122));
#30299=CARTESIAN_POINT('Ctrl Pts',(-188.926861534792,91.9791409821367,7.41897832366544));
#30300=CARTESIAN_POINT('',(0.,0.,0.));
#30301=CARTESIAN_POINT('Origin',(-69.4209305758952,-120.,-82.5));
#30302=CARTESIAN_POINT('',(-69.4209305758952,-120.,-89.25));
#30303=CARTESIAN_POINT('Origin',(-69.4209305758952,-120.,-82.5));
#30304=CARTESIAN_POINT('',(-69.4209305758952,-115.,-89.25));
#30305=CARTESIAN_POINT('',(-69.4209305758952,-120.,-89.25));
#30306=CARTESIAN_POINT('Origin',(-69.4209305758952,-115.,-82.5));
#30307=CARTESIAN_POINT('Origin',(-69.4209305758952,-120.,-247.5));
#30308=CARTESIAN_POINT('',(-69.4209305758952,-120.,-254.25));
#30309=CARTESIAN_POINT('Origin',(-69.4209305758952,-120.,-247.5));
#30310=CARTESIAN_POINT('',(-69.4209305758952,-115.,-254.25));
#30311=CARTESIAN_POINT('',(-69.4209305758952,-120.,-254.25));
#30312=CARTESIAN_POINT('Origin',(-69.4209305758952,-115.,-247.5));
#30313=CARTESIAN_POINT('Origin',(69.4209305758952,-120.,-247.5));
#30314=CARTESIAN_POINT('',(69.4209305758952,-120.,-254.25));
#30315=CARTESIAN_POINT('Origin',(69.4209305758952,-120.,-247.5));
#30316=CARTESIAN_POINT('',(69.4209305758952,-115.,-254.25));
#30317=CARTESIAN_POINT('',(69.4209305758952,-120.,-254.25));
#30318=CARTESIAN_POINT('Origin',(69.4209305758952,-115.,-247.5));
#30319=CARTESIAN_POINT('Origin',(69.4209305758952,-120.,-82.5));
#30320=CARTESIAN_POINT('',(69.4209305758952,-120.,-89.25));
#30321=CARTESIAN_POINT('Origin',(69.4209305758952,-120.,-82.5));
#30322=CARTESIAN_POINT('',(69.4209305758952,-115.,-89.25));
#30323=CARTESIAN_POINT('',(69.4209305758952,-120.,-89.25));
#30324=CARTESIAN_POINT('Origin',(69.4209305758952,-115.,-82.5));
#30325=CARTESIAN_POINT('Origin',(95.,0.,1.06911941042124E-14));
#30326=CARTESIAN_POINT('',(95.,-257.272114237069,42.3824489701997));
#30327=CARTESIAN_POINT('',(95.,-391.404841890133,42.3824489701997));
#30328=CARTESIAN_POINT('',(95.,-250.,42.3824489701997));
#30329=CARTESIAN_POINT('',(95.0000000000001,-257.272114237069,-444.538560851304));
#30330=CARTESIAN_POINT('',(95.,-257.272114237069,42.3824489701998));
#30331=CARTESIAN_POINT('',(95.0000000000001,-250.,-444.538560851304));
#30332=CARTESIAN_POINT('',(95.0000000000001,-250.,-444.538560851304));
#30333=CARTESIAN_POINT('',(95.,-250.,-55.9088729914395));
#30334=CARTESIAN_POINT('',(95.,-250.,42.3824489701998));
#30335=CARTESIAN_POINT('',(95.,-115.,-55.9088729914395));
#30336=CARTESIAN_POINT('',(95.,-250.,-55.9088729914395));
#30337=CARTESIAN_POINT('',(95.,-115.,-65.));
#30338=CARTESIAN_POINT('',(95.,-115.,-55.9088729914395));
#30339=CARTESIAN_POINT('',(95.,-120.,-65.));
#30340=CARTESIAN_POINT('',(95.,-120.,-65.));
#30341=CARTESIAN_POINT('',(95.,-120.,-265.));
#30342=CARTESIAN_POINT('',(95.,-120.,-65.));
#30343=CARTESIAN_POINT('',(95.,-115.,-265.));
#30344=CARTESIAN_POINT('',(95.,-120.,-265.));
#30345=CARTESIAN_POINT('',(95.0000000000001,-284.055947712418,-511.630980392157));
#30346=CARTESIAN_POINT('',(95.0000000000001,-284.055947712418,-511.630980392157));
#30347=CARTESIAN_POINT('',(95.0000000000001,-391.404841890133,-511.630980392157));
#30348=CARTESIAN_POINT('',(95.0000000000001,-391.404841890133,-511.630980392157));
#30349=CARTESIAN_POINT('',(95.,-391.404841890133,42.3824489701997));
#30350=CARTESIAN_POINT('Origin',(-95.,0.,1.06911941042124E-14));
#30351=CARTESIAN_POINT('',(-95.0000000000001,-257.272114237069,-444.538560851304));
#30352=CARTESIAN_POINT('',(-95.0000000000001,-250.,-444.538560851304));
#30353=CARTESIAN_POINT('',(-95.,-250.,-444.538560851304));
#30354=CARTESIAN_POINT('',(-95.,-257.272114237069,42.3824489701997));
#30355=CARTESIAN_POINT('',(-95.,-257.272114237069,42.3824489701996));
#30356=CARTESIAN_POINT('',(-95.,-391.404841890133,42.3824489701997));
#30357=CARTESIAN_POINT('',(-95.,-250.,42.3824489701997));
#30358=CARTESIAN_POINT('',(-95.0000000000001,-391.404841890133,-511.630980392157));
#30359=CARTESIAN_POINT('',(-95.,-391.404841890133,42.3824489701997));
#30360=CARTESIAN_POINT('',(-95.0000000000001,-284.055947712418,-511.630980392157));
#30361=CARTESIAN_POINT('',(-95.0000000000001,-391.404841890133,-511.630980392157));
#30362=CARTESIAN_POINT('',(-95.,-115.,-265.));
#30363=CARTESIAN_POINT('',(-95.0000000000001,-284.055947712418,-511.630980392157));
#30364=CARTESIAN_POINT('',(-95.,-120.,-265.));
#30365=CARTESIAN_POINT('',(-95.,-120.,-265.));
#30366=CARTESIAN_POINT('',(-95.,-120.,-65.));
#30367=CARTESIAN_POINT('',(-95.,-120.,-265.));
#30368=CARTESIAN_POINT('',(-95.,-115.,-65.));
#30369=CARTESIAN_POINT('',(-95.,-120.,-65.));
#30370=CARTESIAN_POINT('',(-95.,-115.,-55.9088729914395));
#30371=CARTESIAN_POINT('',(-95.,-115.,-55.9088729914395));
#30372=CARTESIAN_POINT('',(-95.,-250.,-55.9088729914395));
#30373=CARTESIAN_POINT('',(-95.,-250.,-55.9088729914395));
#30374=CARTESIAN_POINT('',(-95.,-250.,42.3824489701996));
#30375=CARTESIAN_POINT('Origin',(39.9999999999999,-120.,-65.));
#30376=CARTESIAN_POINT('',(39.9999999999999,-115.,-65.));
#30377=CARTESIAN_POINT('',(39.9999999999999,-115.,-65.));
#30378=CARTESIAN_POINT('',(39.9999999999999,-120.,-65.));
#30379=CARTESIAN_POINT('',(39.9999999999999,-120.,-65.));
#30380=CARTESIAN_POINT('',(39.9999999999999,-120.,-65.));
#30381=CARTESIAN_POINT('Origin',(39.9999999999999,-120.,-137.));
#30382=CARTESIAN_POINT('',(39.9999999999999,-115.,-137.));
#30383=CARTESIAN_POINT('',(39.9999999999999,-115.,-137.));
#30384=CARTESIAN_POINT('',(39.9999999999999,-120.,-137.));
#30385=CARTESIAN_POINT('',(39.9999999999999,-120.,-137.));
#30386=CARTESIAN_POINT('',(39.9999999999999,-120.,-137.));
#30387=CARTESIAN_POINT('Origin',(-40.0000000000001,-120.,-137.));
#30388=CARTESIAN_POINT('',(-40.0000000000001,-115.,-137.));
#30389=CARTESIAN_POINT('',(-40.0000000000001,-115.,-137.));
#30390=CARTESIAN_POINT('',(-40.0000000000001,-120.,-137.));
#30391=CARTESIAN_POINT('',(-40.0000000000001,-120.,-137.));
#30392=CARTESIAN_POINT('',(-40.0000000000001,-120.,-137.));
#30393=CARTESIAN_POINT('Origin',(-40.0000000000001,-120.,-65.));
#30394=CARTESIAN_POINT('',(-40.0000000000001,-115.,-65.));
#30395=CARTESIAN_POINT('',(-40.0000000000001,-115.,-65.));
#30396=CARTESIAN_POINT('',(-40.0000000000001,-120.,-65.));
#30397=CARTESIAN_POINT('',(-40.0000000000001,-120.,-65.));
#30398=CARTESIAN_POINT('',(-40.0000000000001,-120.,-65.));
#30399=CARTESIAN_POINT('Origin',(-95.,-120.,-65.));
#30400=CARTESIAN_POINT('',(-95.,-115.,-65.));
#30401=CARTESIAN_POINT('',(-95.,-120.,-65.));
#30402=CARTESIAN_POINT('Origin',(-40.0000000000001,-120.,-265.));
#30403=CARTESIAN_POINT('',(-40.0000000000001,-115.,-265.));
#30404=CARTESIAN_POINT('',(-40.0000000000001,-115.,-265.));
#30405=CARTESIAN_POINT('',(-40.0000000000001,-120.,-265.));
#30406=CARTESIAN_POINT('',(-40.0000000000001,-120.,-265.));
#30407=CARTESIAN_POINT('',(-40.0000000000001,-120.,-265.));
#30408=CARTESIAN_POINT('Origin',(-40.0000000000001,-120.,-189.23552392847));
#30409=CARTESIAN_POINT('',(-40.0000000000001,-115.,-189.23552392847));
#30410=CARTESIAN_POINT('',(-40.0000000000001,-115.,-189.23552392847));
#30411=CARTESIAN_POINT('',(-40.0000000000001,-120.,-189.23552392847));
#30412=CARTESIAN_POINT('',(-40.0000000000001,-120.,-189.23552392847));
#30413=CARTESIAN_POINT('',(-40.0000000000001,-120.,-189.23552392847));
#30414=CARTESIAN_POINT('Origin',(39.9999999999999,-120.,-189.23552392847));
#30415=CARTESIAN_POINT('',(39.9999999999999,-115.,-189.23552392847));
#30416=CARTESIAN_POINT('',(39.9999999999999,-115.,-189.23552392847));
#30417=CARTESIAN_POINT('',(39.9999999999999,-120.,-189.23552392847));
#30418=CARTESIAN_POINT('',(39.9999999999999,-120.,-189.23552392847));
#30419=CARTESIAN_POINT('',(39.9999999999999,-120.,-189.23552392847));
#30420=CARTESIAN_POINT('Origin',(39.9999999999999,-120.,-265.));
#30421=CARTESIAN_POINT('',(39.9999999999999,-115.,-265.));
#30422=CARTESIAN_POINT('',(39.9999999999999,-115.,-265.));
#30423=CARTESIAN_POINT('',(39.9999999999999,-120.,-265.));
#30424=CARTESIAN_POINT('',(39.9999999999999,-120.,-265.));
#30425=CARTESIAN_POINT('',(39.9999999999999,-120.,-265.));
#30426=CARTESIAN_POINT('Origin',(95.,-120.,-265.));
#30427=CARTESIAN_POINT('',(95.,-115.,-265.));
#30428=CARTESIAN_POINT('',(95.,-120.,-265.));
#30429=CARTESIAN_POINT('Origin',(0.,-120.,0.));
#30430=CARTESIAN_POINT('Origin',(0.,-115.,0.));
#30431=CARTESIAN_POINT('',(100.,-115.,-55.9088729914395));
#30432=CARTESIAN_POINT('',(100.,-115.,-55.9088729914395));
#30433=CARTESIAN_POINT('',(100.,-115.,-265.));
#30434=CARTESIAN_POINT('',(100.,-115.,-55.9088729914395));
#30435=CARTESIAN_POINT('',(100.,-115.,-265.));
#30436=CARTESIAN_POINT('',(-100.,-115.,-265.));
#30437=CARTESIAN_POINT('',(-100.,-115.,-265.));
#30438=CARTESIAN_POINT('',(-100.,-115.,-55.9088729914395));
#30439=CARTESIAN_POINT('',(-100.,-115.,-55.9088729914395));
#30440=CARTESIAN_POINT('',(-100.,-115.,-55.9088729914395));
#30441=CARTESIAN_POINT('Origin',(100.,-284.055947712418,-511.630980392157));
#30442=CARTESIAN_POINT('',(100.,-284.055947712418,-511.630980392157));
#30443=CARTESIAN_POINT('',(100.,-284.055947712418,-511.630980392157));
#30444=CARTESIAN_POINT('',(100.,-284.055947712418,-511.630980392157));
#30445=CARTESIAN_POINT('Origin',(100.,-250.,-55.9088729914395));
#30446=CARTESIAN_POINT('',(100.,-250.,-55.9088729914395));
#30447=CARTESIAN_POINT('',(100.,-250.,-55.9088729914395));
#30448=CARTESIAN_POINT('',(100.,-250.,-55.9088729914395));
#30449=CARTESIAN_POINT('Origin',(100.,-250.,-55.9088729914395));
#30450=CARTESIAN_POINT('',(-581.975310925584,-250.,-444.538560851304));
#30451=CARTESIAN_POINT('',(-100.,-250.,-55.9088729914395));
#30452=CARTESIAN_POINT('',(-100.,-250.,-55.9088729914395));
#30453=CARTESIAN_POINT('',(-100.,-250.,42.3824489701997));
#30454=CARTESIAN_POINT('',(-100.,-250.,-55.9088729914395));
#30455=CARTESIAN_POINT('',(100.,-250.,42.3824489701997));
#30456=CARTESIAN_POINT('',(100.,-250.,42.3824489701997));
#30457=CARTESIAN_POINT('',(100.,-250.,-55.9088729914395));
#30458=CARTESIAN_POINT('Origin',(100.,-250.,42.3824489701997));
#30459=CARTESIAN_POINT('',(-100.,-391.404841890133,42.3824489701997));
#30460=CARTESIAN_POINT('',(-100.,-250.,42.3824489701997));
#30461=CARTESIAN_POINT('',(-100.,-391.404841890133,42.3824489701997));
#30462=CARTESIAN_POINT('',(-581.975310925585,-257.272114237069,42.3824489701997));
#30463=CARTESIAN_POINT('',(100.,-391.404841890133,42.3824489701997));
#30464=CARTESIAN_POINT('',(100.,-391.404841890133,42.3824489701997));
#30465=CARTESIAN_POINT('',(100.,-250.,42.3824489701997));
#30466=CARTESIAN_POINT('Origin',(100.,-391.404841890133,42.3824489701997));
#30467=CARTESIAN_POINT('',(100.,-391.404841890133,-511.630980392157));
#30468=CARTESIAN_POINT('',(100.,-391.404841890133,-511.630980392157));
#30469=CARTESIAN_POINT('',(100.,-391.404841890133,42.3824489701997));
#30470=CARTESIAN_POINT('Origin',(100.,-391.404841890133,-511.630980392157));
#30471=CARTESIAN_POINT('',(100.,-391.404841890133,-511.630980392157));
#30472=CARTESIAN_POINT('Origin',(100.,0.,1.13850834946031E-14));
#30473=CARTESIAN_POINT('Origin',(-100.,-284.055947712418,-511.630980392157));
#30474=CARTESIAN_POINT('',(-100.,-284.055947712418,-511.630980392157));
#30475=CARTESIAN_POINT('',(-100.,-284.055947712418,-511.630980392157));
#30476=CARTESIAN_POINT('',(-100.,-284.055947712418,-511.630980392157));
#30477=CARTESIAN_POINT('Origin',(-100.,-391.404841890133,-511.630980392157));
#30478=CARTESIAN_POINT('',(-100.,-391.404841890133,-511.630980392157));
#30479=CARTESIAN_POINT('',(-100.,-391.404841890133,-511.630980392157));
#30480=CARTESIAN_POINT('',(-100.,-391.404841890133,-511.630980392157));
#30481=CARTESIAN_POINT('Origin',(-100.,-391.404841890133,42.3824489701997));
#30482=CARTESIAN_POINT('',(-100.,-391.404841890133,42.3824489701997));
#30483=CARTESIAN_POINT('Origin',(-100.,-250.,-55.9088729914395));
#30484=CARTESIAN_POINT('',(-100.,-250.,-55.9088729914395));
#30485=CARTESIAN_POINT('Origin',(-100.,0.,1.13850834946031E-14));
#30486=CARTESIAN_POINT('Origin',(-581.975310925585,-257.272114237069,42.3824489701997));
#30487=CARTESIAN_POINT('',(-581.975310925584,-257.272114237069,-444.538560851304));
#30488=CARTESIAN_POINT('Origin',(-581.975310925584,-250.,-444.538560851304));
#30489=CARTESIAN_POINT('',(0.,0.,0.));
#30490=CARTESIAN_POINT('Origin',(-143.851228669208,0.,55.));
#30491=CARTESIAN_POINT('',(-240.012422008234,-1.17763497624828E-14,55.));
#30492=CARTESIAN_POINT('Origin',(-143.851228669208,0.,55.));
#30493=CARTESIAN_POINT('',(-240.012422008234,-1.17763497624828E-14,60.));
#30494=CARTESIAN_POINT('',(-240.012422008234,-1.17763497624828E-14,55.));
#30495=CARTESIAN_POINT('Origin',(-143.851228669208,0.,60.));
#30496=CARTESIAN_POINT('Origin',(0.,267.,60.));
#30497=CARTESIAN_POINT('',(2.5,267.,60.));
#30498=CARTESIAN_POINT('Origin',(0.,267.,60.));
#30499=CARTESIAN_POINT('',(2.5,267.,55.));
#30500=CARTESIAN_POINT('',(2.5,267.,60.));
#30501=CARTESIAN_POINT('Origin',(0.,267.,55.));
#30502=CARTESIAN_POINT('Origin',(108.598683701239,243.916637190574,60.));
#30503=CARTESIAN_POINT('',(111.098683701239,243.916637190574,60.));
#30504=CARTESIAN_POINT('Origin',(108.598683701239,243.916637190574,60.));
#30505=CARTESIAN_POINT('',(111.098683701239,243.916637190574,55.));
#30506=CARTESIAN_POINT('',(111.098683701239,243.916637190574,60.));
#30507=CARTESIAN_POINT('Origin',(108.598683701239,243.916637190574,55.));
#30508=CARTESIAN_POINT('Origin',(198.419668402464,178.657871897815,60.));
#30509=CARTESIAN_POINT('',(200.919668402464,178.657871897815,60.));
#30510=CARTESIAN_POINT('Origin',(198.419668402464,178.657871897815,60.));
#30511=CARTESIAN_POINT('',(200.919668402464,178.657871897815,55.));
#30512=CARTESIAN_POINT('',(200.919668402464,178.657871897815,60.));
#30513=CARTESIAN_POINT('Origin',(198.419668402464,178.657871897815,55.));
#30514=CARTESIAN_POINT('Origin',(253.932089850806,82.507537498111,60.));
#30515=CARTESIAN_POINT('',(256.432089850806,82.507537498111,60.));
#30516=CARTESIAN_POINT('Origin',(253.932089850806,82.507537498111,60.));
#30517=CARTESIAN_POINT('',(256.432089850806,82.507537498111,55.));
#30518=CARTESIAN_POINT('',(256.432089850806,82.507537498111,60.));
#30519=CARTESIAN_POINT('Origin',(253.932089850806,82.507537498111,55.));
#30520=CARTESIAN_POINT('Origin',(265.537346063329,-27.9090996924634,60.));
#30521=CARTESIAN_POINT('',(268.037346063329,-27.9090996924634,60.));
#30522=CARTESIAN_POINT('Origin',(265.537346063329,-27.9090996924634,60.));
#30523=CARTESIAN_POINT('',(268.037346063329,-27.9090996924634,55.));
#30524=CARTESIAN_POINT('',(268.037346063329,-27.9090996924634,60.));
#30525=CARTESIAN_POINT('Origin',(265.537346063329,-27.9090996924634,55.));
#30526=CARTESIAN_POINT('Origin',(231.228782810445,-133.5,60.));
#30527=CARTESIAN_POINT('',(233.728782810445,-133.5,60.));
#30528=CARTESIAN_POINT('Origin',(231.228782810445,-133.5,60.));
#30529=CARTESIAN_POINT('',(233.728782810445,-133.5,55.));
#30530=CARTESIAN_POINT('',(233.728782810445,-133.5,60.));
#30531=CARTESIAN_POINT('Origin',(231.228782810445,-133.5,55.));
#30532=CARTESIAN_POINT('Origin',(156.93866236209,-216.007537498111,60.));
#30533=CARTESIAN_POINT('',(159.43866236209,-216.007537498111,60.));
#30534=CARTESIAN_POINT('Origin',(156.93866236209,-216.007537498111,60.));
#30535=CARTESIAN_POINT('',(159.43866236209,-216.007537498111,55.));
#30536=CARTESIAN_POINT('',(159.43866236209,-216.007537498111,60.));
#30537=CARTESIAN_POINT('Origin',(156.93866236209,-216.007537498111,55.));
#30538=CARTESIAN_POINT('Origin',(55.5124214483419,-261.165409395926,60.));
#30539=CARTESIAN_POINT('',(58.0124214483419,-261.165409395926,60.));
#30540=CARTESIAN_POINT('Origin',(55.5124214483419,-261.165409395926,60.));
#30541=CARTESIAN_POINT('',(58.0124214483419,-261.165409395926,55.));
#30542=CARTESIAN_POINT('',(58.0124214483419,-261.165409395926,60.));
#30543=CARTESIAN_POINT('Origin',(55.5124214483419,-261.165409395926,55.));
#30544=CARTESIAN_POINT('Origin',(-55.5124214483417,-261.165409395926,60.));
#30545=CARTESIAN_POINT('',(-53.0124214483417,-261.165409395926,60.));
#30546=CARTESIAN_POINT('Origin',(-55.5124214483417,-261.165409395926,60.));
#30547=CARTESIAN_POINT('',(-53.0124214483417,-261.165409395926,55.));
#30548=CARTESIAN_POINT('',(-53.0124214483417,-261.165409395926,60.));
#30549=CARTESIAN_POINT('Origin',(-55.5124214483417,-261.165409395926,55.));
#30550=CARTESIAN_POINT('Origin',(-156.93866236209,-216.007537498111,60.));
#30551=CARTESIAN_POINT('',(-154.43866236209,-216.007537498111,60.));
#30552=CARTESIAN_POINT('Origin',(-156.93866236209,-216.007537498111,60.));
#30553=CARTESIAN_POINT('',(-154.43866236209,-216.007537498111,55.));
#30554=CARTESIAN_POINT('',(-154.43866236209,-216.007537498111,60.));
#30555=CARTESIAN_POINT('Origin',(-156.93866236209,-216.007537498111,55.));
#30556=CARTESIAN_POINT('Origin',(-231.228782810445,-133.5,60.));
#30557=CARTESIAN_POINT('',(-228.728782810445,-133.5,60.));
#30558=CARTESIAN_POINT('Origin',(-231.228782810445,-133.5,60.));
#30559=CARTESIAN_POINT('',(-228.728782810445,-133.5,55.));
#30560=CARTESIAN_POINT('',(-228.728782810445,-133.5,60.));
#30561=CARTESIAN_POINT('Origin',(-231.228782810445,-133.5,55.));
#30562=CARTESIAN_POINT('Origin',(-265.537346063329,-27.9090996924637,60.));
#30563=CARTESIAN_POINT('',(-263.037346063329,-27.9090996924637,60.));
#30564=CARTESIAN_POINT('Origin',(-265.537346063329,-27.9090996924637,60.));
#30565=CARTESIAN_POINT('',(-263.037346063329,-27.9090996924637,55.));
#30566=CARTESIAN_POINT('',(-263.037346063329,-27.9090996924637,60.));
#30567=CARTESIAN_POINT('Origin',(-265.537346063329,-27.9090996924637,55.));
#30568=CARTESIAN_POINT('Origin',(-253.932089850806,82.5075374981109,60.));
#30569=CARTESIAN_POINT('',(-251.432089850806,82.5075374981109,60.));
#30570=CARTESIAN_POINT('Origin',(-253.932089850806,82.5075374981109,60.));
#30571=CARTESIAN_POINT('',(-251.432089850806,82.5075374981109,55.));
#30572=CARTESIAN_POINT('',(-251.432089850806,82.5075374981109,60.));
#30573=CARTESIAN_POINT('Origin',(-253.932089850806,82.5075374981109,55.));
#30574=CARTESIAN_POINT('Origin',(-198.419668402464,178.657871897815,60.));
#30575=CARTESIAN_POINT('',(-195.919668402464,178.657871897815,60.));
#30576=CARTESIAN_POINT('Origin',(-198.419668402464,178.657871897815,60.));
#30577=CARTESIAN_POINT('',(-195.919668402464,178.657871897815,55.));
#30578=CARTESIAN_POINT('',(-195.919668402464,178.657871897815,60.));
#30579=CARTESIAN_POINT('Origin',(-198.419668402464,178.657871897815,55.));
#30580=CARTESIAN_POINT('Origin',(-108.598683701239,243.916637190575,60.));
#30581=CARTESIAN_POINT('',(-106.098683701239,243.916637190575,60.));
#30582=CARTESIAN_POINT('Origin',(-108.598683701239,243.916637190575,60.));
#30583=CARTESIAN_POINT('',(-106.098683701239,243.916637190575,55.));
#30584=CARTESIAN_POINT('',(-106.098683701239,243.916637190575,60.));
#30585=CARTESIAN_POINT('Origin',(-108.598683701239,243.916637190575,55.));
#30586=CARTESIAN_POINT('Origin',(0.,0.,60.));
#30587=CARTESIAN_POINT('',(275.,-3.36777869765522E-14,55.));
#30588=CARTESIAN_POINT('Origin',(0.,0.,55.));
#30589=CARTESIAN_POINT('',(275.,-3.36777869765522E-14,60.));
#30590=CARTESIAN_POINT('',(275.,-3.36777869765522E-14,60.));
#30591=CARTESIAN_POINT('Origin',(0.,0.,60.));
#30592=CARTESIAN_POINT('Origin',(0.,0.,60.));
#30593=CARTESIAN_POINT('Origin',(0.,0.,55.));
#30594=CARTESIAN_POINT('Origin',(-143.851228669208,0.,55.));
#30595=CARTESIAN_POINT('',(-240.012422008234,-1.17763497624828E-14,60.));
#30596=CARTESIAN_POINT('Origin',(-143.851228669208,0.,60.));
#30597=CARTESIAN_POINT('',(-240.012422008234,-1.17763497624828E-14,55.));
#30598=CARTESIAN_POINT('',(-240.012422008234,-1.17763497624828E-14,55.));
#30599=CARTESIAN_POINT('Origin',(-143.851228669208,0.,55.));
#30600=CARTESIAN_POINT('Origin',(-143.851228669208,0.,55.));
#30601=CARTESIAN_POINT('Origin',(-143.851228669208,0.,60.));
#30602=CARTESIAN_POINT('',(0.,0.,0.));
#30603=CARTESIAN_POINT('Origin',(1.3944401189292E-12,-11.1689999999806,
-178.099999999984));
#30604=CARTESIAN_POINT('',(-25.3339394440343,-11.168999999981,-181.499999999985));
#30605=CARTESIAN_POINT('Origin',(1.04025109975431E-12,-11.168999999981,
-181.499999999985));
#30606=CARTESIAN_POINT('',(-27.3317482398788,-11.1689999999812,-182.813484492891));
#30607=CARTESIAN_POINT('Origin',(-28.9999999999993,-11.1689999999806,-178.099999999984));
#30608=CARTESIAN_POINT('',(-1.27149462683012E-12,16.1627482398987,-182.813484492894));
#30609=CARTESIAN_POINT('Origin',(1.11022302462516E-12,-11.1689999999811,
-182.813484492891));
#30610=CARTESIAN_POINT('Origin',(1.11022302462516E-12,-11.1689999999811,
-182.813484492891));
#30611=CARTESIAN_POINT('Origin',(3.84137166520304E-13,-11.1689999999818,
-187.999999999984));
#30612=CARTESIAN_POINT('',(-28.668251760119,-11.1689999999812,-183.286515507081));
#30613=CARTESIAN_POINT('',(-1.38795896703444E-12,17.4992517601389,-183.286515507084));
#30614=CARTESIAN_POINT('Origin',(1.11022302462516E-12,-11.1689999999812,
-183.286515507081));
#30615=CARTESIAN_POINT('',(-29.757543650104,-11.1689999999813,-183.829154400138));
#30616=CARTESIAN_POINT('Origin',(-27.0000000000005,-11.1689999999818,-187.999999999984));
#30617=CARTESIAN_POINT('',(-1.48288102248418E-12,18.5885436501236,-183.829154400142));
#30618=CARTESIAN_POINT('Origin',(1.11022302462516E-12,-11.1689999999813,
-183.829154400138));
#30619=CARTESIAN_POINT('Origin',(1.11022302462516E-12,-11.1689999999813,
-183.829154400138));
#30620=CARTESIAN_POINT('Origin',(1.11022302462516E-12,-11.1689999999812,
-183.286515507081));
#30621=CARTESIAN_POINT('Origin',(1.21236354289067E-12,-11.1689999999812,
-182.999999999985));
#30622=CARTESIAN_POINT('',(-45.3097394023371,-11.1689999999816,-186.995472550883));
#30623=CARTESIAN_POINT('',(-2.8381159242873E-12,34.1407394023565,-186.995472550889));
#30624=CARTESIAN_POINT('Origin',(1.11022302462516E-12,-11.1689999999816,
-186.995472550883));
#30625=CARTESIAN_POINT('',(-49.0555555555546,-11.1689999999814,-184.832491389149));
#30626=CARTESIAN_POINT('Origin',(-45.4999999999988,-11.1689999999812,-182.999999999985));
#30627=CARTESIAN_POINT('',(5.42612633001892E-12,-60.2245555555371,-184.832491389143));
#30628=CARTESIAN_POINT('Origin',(1.11022302462516E-12,-11.1689999999814,
-184.832491389149));
#30629=CARTESIAN_POINT('Origin',(1.11022302462516E-12,-11.1689999999814,
-184.832491389149));
#30630=CARTESIAN_POINT('Origin',(1.11022302462516E-12,-11.1689999999816,
-186.995472550883));
#30631=CARTESIAN_POINT('Origin',(2.33812968986058E-12,-11.1689999999812,
-182.499999999986));
#30632=CARTESIAN_POINT('',(-32.7939650799149,-11.1689999999816,-185.836676479864));
#30633=CARTESIAN_POINT('',(-1.74747801983562E-12,21.6249650799345,-185.836676479867));
#30634=CARTESIAN_POINT('Origin',(1.11022302462516E-12,-11.1689999999815,
-185.836676479864));
#30635=CARTESIAN_POINT('',(-34.8097394023371,-11.1689999999817,-186.495472550884));
#30636=CARTESIAN_POINT('Origin',(-34.9999999999981,-11.1689999999812,-182.499999999986));
#30637=CARTESIAN_POINT('',(-1.92313474120327E-12,23.6407394023566,-186.495472550887));
#30638=CARTESIAN_POINT('Origin',(1.11022302462516E-12,-11.1689999999816,
-186.495472550884));
#30639=CARTESIAN_POINT('Origin',(1.11022302462516E-12,-11.1689999999816,
-186.495472550884));
#30640=CARTESIAN_POINT('Origin',(1.11022302462516E-12,-11.1689999999815,
-185.836676479864));
#30641=CARTESIAN_POINT('Origin',(1.11022302462516E-12,-11.1689999999813,
-183.999999999986));
#30642=CARTESIAN_POINT('',(5.91645271747501E-12,-66.1689999999812,-182.999999999979));
#30643=CARTESIAN_POINT('Origin',(1.12277548732324E-12,-11.1689999999812,
-182.999999999985));
#30644=CARTESIAN_POINT('',(5.91645271747499E-12,-66.168999999981,-181.499999999979));
#30645=CARTESIAN_POINT('',(5.91645271747502E-12,-66.1689999999813,-183.999999999979));
#30646=CARTESIAN_POINT('Origin',(1.11910480882216E-12,-11.168999999981,
-181.499999999985));
#30647=CARTESIAN_POINT('Origin',(1.11022302462516E-12,-11.1689999999812,
-183.286515507081));
#30648=CARTESIAN_POINT('',(-1.38795896703444E-12,17.4992517601389,-183.286515507084));
#30649=CARTESIAN_POINT('Origin',(1.11022302462516E-12,-11.1689999999812,
-182.999999999985));
#30650=CARTESIAN_POINT('',(5.4678483962789E-12,-61.1689999999812,-182.999999999979));
#30651=CARTESIAN_POINT('',(5.47952274539776E-12,-61.1689999999812,-182.99999999998));
#30652=CARTESIAN_POINT('Origin',(1.10617921426542E-12,-11.1689999999812,
-182.999999999985));
#30653=CARTESIAN_POINT('Origin',(1.11022302462516E-12,-11.1689999999815,
-185.836676479864));
#30654=CARTESIAN_POINT('',(-1.74747801983562E-12,21.6249650799345,-185.836676479867));
#30655=CARTESIAN_POINT('Origin',(1.11022302462516E-12,-11.1689999999816,
-186.995472550884));
#30656=CARTESIAN_POINT('',(-2.8381159242873E-12,34.1407394023566,-186.995472550889));
#30657=CARTESIAN_POINT('Origin',(1.11022302462516E-12,-11.168999999981,
-181.499999999986));
#30658=CARTESIAN_POINT('Origin',(-54.9999999999989,-11.168999999986,-182.999999999985));
#30659=CARTESIAN_POINT('Origin',(-6.0507154842071E-12,70.6167142857329,
-355.499999999994));
#30660=CARTESIAN_POINT('',(-6.03542612711786E-12,70.616714285733,-354.642857142845));
#30661=CARTESIAN_POINT('',(-6.04778737592304E-12,70.6167142857215,-356.357142857121));
#30662=CARTESIAN_POINT('Origin',(-6.0507154842071E-12,70.6167142857329,
-355.499999999994));
#30663=CARTESIAN_POINT('Origin',(-6.0507154842071E-12,70.6167142857329,
-355.499999999994));
#30664=CARTESIAN_POINT('',(-6.02295990859147E-12,70.3310000000051,-354.699999999991));
#30665=CARTESIAN_POINT('',(-6.05061051448147E-12,70.616714285733,-354.642857142845));
#30666=CARTESIAN_POINT('Origin',(-6.0278687718437E-12,70.3310000000051,
-355.499999999995));
#30667=CARTESIAN_POINT('Origin',(-6.02295990859147E-12,70.3310000001228,
-355.499999999994));
#30668=CARTESIAN_POINT('',(-6.02295990859147E-12,70.3310000000504,-356.499999999962));
#30669=CARTESIAN_POINT('',(-6.02283744391155E-12,70.3310000001227,-356.49999999992));
#30670=CARTESIAN_POINT('Origin',(-6.03053145953967E-12,70.3310000000491,
-355.499999999995));
#30671=CARTESIAN_POINT('Origin',(-42.5000000000061,70.331,-312.999999999994));
#30672=CARTESIAN_POINT('Origin',(-6.10622663543836E-12,71.3310000000423,
-355.499999999994));
#30673=CARTESIAN_POINT('',(-6.1934901652352E-12,72.3310000007449,-355.499999999995));
#30674=CARTESIAN_POINT('',(-6.10622663543836E-12,71.3309999999794,-356.));
#30675=CARTESIAN_POINT('',(-6.1061654030984E-12,71.3310000000423,-355.999999999961));
#30676=CARTESIAN_POINT('Origin',(-6.10622663543457E-12,71.3309999999989,
-355.499999999994));
#30677=CARTESIAN_POINT('Origin',(-6.10622663543836E-12,71.3309999999989,
-355.499999999994));
#30678=CARTESIAN_POINT('Origin',(-88.2,2.21370231173746E-11,-87.4999999999866));
#30679=CARTESIAN_POINT('',(-88.2,-1.44337567297757,-84.9999999999864));
#30680=CARTESIAN_POINT('',(-88.2,-2.88675134587786,-87.4999999999863));
#30681=CARTESIAN_POINT('',(-88.2,-1.44337567297757,-84.9999999999864));
#30682=CARTESIAN_POINT('',(-88.2,-1.44337567297815,-89.9999999999864));
#30683=CARTESIAN_POINT('',(-88.2,-2.88675134587786,-87.4999999999863));
#30684=CARTESIAN_POINT('',(-88.2,1.44337567302184,-89.9999999999867));
#30685=CARTESIAN_POINT('',(-88.2,2.18594673612182E-11,-89.9999999999866));
#30686=CARTESIAN_POINT('',(-88.2,2.88675134592214,-87.4999999999869));
#30687=CARTESIAN_POINT('',(-88.2,1.44337567302184,-89.9999999999867));
#30688=CARTESIAN_POINT('',(-88.2,1.44337567302243,-84.9999999999868));
#30689=CARTESIAN_POINT('',(-88.2,2.88675134592214,-87.4999999999869));
#30690=CARTESIAN_POINT('',(-88.2,2.24145788735308E-11,-84.9999999999866));
#30691=CARTESIAN_POINT('Origin',(-88.2,-2.165063509428,-88.7499999999863));
#30692=CARTESIAN_POINT('',(-85.,-1.44337567297788,-89.9999999999864));
#30693=CARTESIAN_POINT('',(-88.2,-1.44337567297815,-89.9999999999864));
#30694=CARTESIAN_POINT('',(-85.,-2.88675134587758,-87.4999999999863));
#30695=CARTESIAN_POINT('',(-88.2,-2.88675134587786,-87.4999999999863));
#30696=CARTESIAN_POINT('',(-85.,-2.16506350942773,-88.7499999999863));
#30697=CARTESIAN_POINT('Origin',(-88.2,-2.16506350942773,-86.2499999999863));
#30698=CARTESIAN_POINT('',(-85.,-1.44337567297729,-84.9999999999864));
#30699=CARTESIAN_POINT('',(-88.2,-1.44337567297757,-84.9999999999864));
#30700=CARTESIAN_POINT('',(-85.,-2.16506350942745,-86.2499999999863));
#30701=CARTESIAN_POINT('Origin',(-88.2,2.24145788735308E-11,-84.9999999999866));
#30702=CARTESIAN_POINT('',(-84.8059326826218,1.44337567302271,-84.9999999999868));
#30703=CARTESIAN_POINT('',(-88.2,1.44337567302243,-84.9999999999868));
#30704=CARTESIAN_POINT('',(-85.,2.26921346296871E-11,-84.9999999999866));
#30705=CARTESIAN_POINT('',(-81.0000000000025,29.7500000000231,-84.99999999999));
#30706=CARTESIAN_POINT('',(-85.,2.26921346296871E-11,-84.9999999999866));
#30707=CARTESIAN_POINT('Origin',(-88.2,2.16506350947228,-86.2499999999868));
#30708=CARTESIAN_POINT('',(-84.6118653652572,2.88675134592244,-87.4999999999869));
#30709=CARTESIAN_POINT('',(-88.2,2.88675134592214,-87.4999999999869));
#30710=CARTESIAN_POINT('',(-84.8059326826218,1.44337567302271,-84.9999999999868));
#30711=CARTESIAN_POINT('Origin',(-88.2,2.165063509472,-88.7499999999868));
#30712=CARTESIAN_POINT('',(-84.8059326826218,1.44337567302212,-89.9999999999867));
#30713=CARTESIAN_POINT('',(-88.2,1.44337567302184,-89.9999999999867));
#30714=CARTESIAN_POINT('',(-84.6118653652572,2.88675134592244,-87.4999999999869));
#30715=CARTESIAN_POINT('Origin',(-88.2,-0.721687836478147,-89.9999999999865));
#30716=CARTESIAN_POINT('',(-85.,2.21092675417589E-11,-89.9999999999866));
#30717=CARTESIAN_POINT('',(-84.8059326826218,1.44337567302212,-89.9999999999867));
#30718=CARTESIAN_POINT('',(-85.,-0.72168783647787,-89.9999999999865));
#30719=CARTESIAN_POINT('Origin',(-84.9999999999949,-57.499999999973,-47.49999999998));
#30720=CARTESIAN_POINT('',(-85.,2.70220044257252E-11,-47.4999999999866));
#30721=CARTESIAN_POINT('Origin',(-81.0000000000025,29.7500000000274,-47.49999999999));
#30722=CARTESIAN_POINT('Ctrl Pts',(41.9445347128706,60.6495679335285,-440.998916834174));
#30723=CARTESIAN_POINT('Ctrl Pts',(31.7948796622976,45.4225605594559,-462.499999999992));
#30724=CARTESIAN_POINT('Ctrl Pts',(47.4083864201783,59.4777499755747,-440.999999999994));
#30725=CARTESIAN_POINT('Ctrl Pts',(34.5033857139737,44.8351009291132,-462.499999999992));
#30726=CARTESIAN_POINT('Ctrl Pts',(52.4006927127278,56.9663054203067,-440.999999999994));
#30727=CARTESIAN_POINT('Ctrl Pts',(36.9523181444856,43.5374708585478,-462.499999999992));
#30728=CARTESIAN_POINT('Ctrl Pts',(56.6023578327675,53.2821982242028,-441.000077522351));
#30729=CARTESIAN_POINT('Ctrl Pts',(38.959068146329,41.6254058239817,-462.499232522636));
#30730=CARTESIAN_POINT('',(56.6023578328014,53.2821982241725,-441.000077522353));
#30731=CARTESIAN_POINT('',(41.945683924215,60.6520270238569,-440.996501147464));
#30732=CARTESIAN_POINT('Ctrl Pts',(56.6023578327675,53.2821982242028,-441.000077522351));
#30733=CARTESIAN_POINT('Ctrl Pts',(52.4008552484363,56.9661629056235,-441.000000002993));
#30734=CARTESIAN_POINT('Ctrl Pts',(47.4087643628648,59.4775598442953,-440.999999999995));
#30735=CARTESIAN_POINT('Ctrl Pts',(41.945141845367,60.649437717353,-440.998916954529));
#30736=CARTESIAN_POINT('',(43.5418850322931,44.6532394080568,-456.914860655543));
#30737=CARTESIAN_POINT('',(56.6023578328014,53.2821982241725,-441.000077522353));
#30738=CARTESIAN_POINT('',(38.7052731678116,41.8608202463478,-462.499996475683));
#30739=CARTESIAN_POINT('Ctrl Pts',(43.5418850322409,44.6532394081205,-456.914860655531));
#30740=CARTESIAN_POINT('Ctrl Pts',(42.6909235753114,44.161936581892,-457.897152546731));
#30741=CARTESIAN_POINT('Ctrl Pts',(41.834968106616,43.6677504616438,-458.885370858913));
#30742=CARTESIAN_POINT('Ctrl Pts',(40.2284919679139,42.740251030517,-460.740479172022));
#30743=CARTESIAN_POINT('Ctrl Pts',(39.4654128251454,42.2996870820088,-461.621826686247));
#30744=CARTESIAN_POINT('Ctrl Pts',(38.7058548823679,41.8611560992808,-462.499324435463));
#30745=CARTESIAN_POINT('',(31.7950297288388,45.4227856965977,-462.499682098234));
#30746=CARTESIAN_POINT('Ctrl Pts',(38.7052701171837,41.8608184850676,-462.499999999996));
#30747=CARTESIAN_POINT('Ctrl Pts',(37.73378223273,42.7450246881099,-462.499999999996));
#30748=CARTESIAN_POINT('Ctrl Pts',(36.6501650229394,43.4975098798192,-462.500000000097));
#30749=CARTESIAN_POINT('Ctrl Pts',(34.3164321736615,44.6996244168636,-462.500000000097));
#30750=CARTESIAN_POINT('Ctrl Pts',(33.0766926857734,45.1445339195995,-462.499999999997));
#30751=CARTESIAN_POINT('Ctrl Pts',(31.794974156998,45.4225400637676,-462.499999999997));
#30752=CARTESIAN_POINT('',(41.9454901388008,60.6510013100927,-440.996892854809));
#30753=CARTESIAN_POINT('Ctrl Pts',(56.6023578327675,53.2821982242028,-441.000077522351));
#30754=CARTESIAN_POINT('Ctrl Pts',(43.5418850322312,44.653239408115,-456.914860655543));
#30755=CARTESIAN_POINT('Ctrl Pts',(59.3135877730366,50.8952105744222,-440.999999999993));
#30756=CARTESIAN_POINT('Ctrl Pts',(47.7405554577269,40.7010682615999,-456.919527671004));
#30757=CARTESIAN_POINT('Ctrl Pts',(61.8717342174682,48.3453380510862,-440.999999999993));
#30758=CARTESIAN_POINT('Ctrl Pts',(51.8201097042108,36.6236615680342,-456.919527671003));
#30759=CARTESIAN_POINT('Ctrl Pts',(64.2705054959308,45.6385004273605,-441.000078147052));
#30760=CARTESIAN_POINT('Ctrl Pts',(55.7738565200363,32.4271120479789,-456.914852766313));
#30761=CARTESIAN_POINT('',(64.2705054959311,45.6385004273602,-441.000078147052));
#30762=CARTESIAN_POINT('Ctrl Pts',(64.2705054959308,45.6385004273605,-441.000078147052));
#30763=CARTESIAN_POINT('Ctrl Pts',(61.8717342174683,48.3453380510863,-440.999999999993));
#30764=CARTESIAN_POINT('Ctrl Pts',(59.3135877730366,50.8952105744222,-440.999999999993));
#30765=CARTESIAN_POINT('Ctrl Pts',(56.6023578327675,53.2821982242028,-441.000077522351));
#30766=CARTESIAN_POINT('',(56.5529890060887,33.6385804635181,-455.455487085885));
#30767=CARTESIAN_POINT('',(64.2705054959311,45.6385004273602,-441.000078147052));
#30768=CARTESIAN_POINT('',(61.00640553759,41.3521241633495,-446.556113667091));
#30769=CARTESIAN_POINT('Ctrl Pts',(56.5529890060882,33.6385804635188,-455.455487085885));
#30770=CARTESIAN_POINT('Ctrl Pts',(57.3013610416582,34.9347988520902,-453.959017905079));
#30771=CARTESIAN_POINT('Ctrl Pts',(58.1247838904071,36.361009062298,-452.312909266844));
#30772=CARTESIAN_POINT('Ctrl Pts',(59.6105260061009,38.9343898936254,-449.34393478218));
#30773=CARTESIAN_POINT('Ctrl Pts',(60.3109178717418,40.1475041900623,-447.944807398955));
#30774=CARTESIAN_POINT('Ctrl Pts',(61.0064055375901,41.3521241633496,-446.556113667091));
#30775=CARTESIAN_POINT('',(52.5211241633506,49.8374055375872,-446.553200603166));
#30776=CARTESIAN_POINT('Ctrl Pts',(61.00640553759,41.3521241633495,-446.556113667092));
#30777=CARTESIAN_POINT('Ctrl Pts',(59.7247235140878,42.8408739671962,-446.491862452654));
#30778=CARTESIAN_POINT('Ctrl Pts',(58.3867645976448,44.2845807962581,-446.459956651753));
#30779=CARTESIAN_POINT('Ctrl Pts',(55.5596333134075,47.1193359090829,-446.456714304226));
#30780=CARTESIAN_POINT('Ctrl Pts',(54.0645693704593,48.508635605192,-446.487617979628));
#30781=CARTESIAN_POINT('Ctrl Pts',(52.5211241633507,49.8374055375873,-446.553200603166));
#30782=CARTESIAN_POINT('Ctrl Pts',(52.5211241633505,49.8374055375871,-446.553200603166));
#30783=CARTESIAN_POINT('Ctrl Pts',(51.1319868849515,49.0353867559617,-448.154229195363));
#30784=CARTESIAN_POINT('Ctrl Pts',(49.7318236496382,48.2270021349601,-449.769111065283));
#30785=CARTESIAN_POINT('Ctrl Pts',(46.7368592415848,46.4978586277563,-453.225121323072));
#30786=CARTESIAN_POINT('Ctrl Pts',(45.0537435888084,45.5261113527318,-455.168522441224));
#30787=CARTESIAN_POINT('Ctrl Pts',(43.5418850322419,44.6532394081211,-456.914860655531));
#30788=CARTESIAN_POINT('Origin',(7.99360577730113E-14,4.65447819175679E-11,
57.5187545213137));
#30789=CARTESIAN_POINT('',(9.75000000013433,4.79819245881191E-11,70.0000000000134));
#30790=CARTESIAN_POINT('Origin',(1.11022302462516E-13,4.79774640155251E-11,
70.0000000000134));
#30791=CARTESIAN_POINT('',(6.7500000000709,4.73830448269764E-11,64.7999999999394));
#30792=CARTESIAN_POINT('Origin',(25.3774921629996,4.65416740711132E-11,
57.5187545213137));
#30793=CARTESIAN_POINT('',(-4.78833159847994E-13,6.75000000011816,64.7999999999386));
#30794=CARTESIAN_POINT('Origin',(1.11022302462516E-13,4.73668413519812E-11,
64.7999999999394));
#30795=CARTESIAN_POINT('Origin',(1.11022302462516E-13,4.73668413519812E-11,
64.7999999999394));
#30796=CARTESIAN_POINT('Origin',(-67.4999999999909,-102.999999999988,-194.999999999975));
#30797=CARTESIAN_POINT('',(-67.4999999999899,-114.999999999988,-188.249999999973));
#30798=CARTESIAN_POINT('Origin',(-67.4999999999899,-114.999999999988,-194.999999999974));
#30799=CARTESIAN_POINT('',(-67.499999999992,-90.9999999999876,-188.249999999976));
#30800=CARTESIAN_POINT('',(-67.4999999999909,-102.999999999988,-188.249999999975));
#30801=CARTESIAN_POINT('Origin',(-67.4999999999919,-90.9999999999884,-194.999999999976));
#30802=CARTESIAN_POINT('Origin',(-67.4999999999909,-102.999999999969,-29.9999999999748));
#30803=CARTESIAN_POINT('',(-67.4999999999899,-114.999999999969,-23.2499999999734));
#30804=CARTESIAN_POINT('Origin',(-67.4999999999899,-114.999999999969,-29.9999999999734));
#30805=CARTESIAN_POINT('',(-67.499999999992,-90.9999999999686,-23.2499999999761));
#30806=CARTESIAN_POINT('',(-67.4999999999909,-102.999999999969,-23.2499999999748));
#30807=CARTESIAN_POINT('Origin',(-67.4999999999919,-90.9999999999694,-29.9999999999761));
#30808=CARTESIAN_POINT('Origin',(67.5000000000091,-102.999999999977,-194.999999999975));
#30809=CARTESIAN_POINT('',(67.5000000000102,-114.999999999976,-188.249999999973));
#30810=CARTESIAN_POINT('Origin',(67.5000000000102,-114.999999999977,-194.999999999974));
#30811=CARTESIAN_POINT('',(67.5000000000081,-90.9999999999759,-188.249999999976));
#30812=CARTESIAN_POINT('',(67.5000000000091,-102.999999999976,-188.249999999975));
#30813=CARTESIAN_POINT('Origin',(67.5000000000081,-90.9999999999767,-194.999999999976));
#30814=CARTESIAN_POINT('Origin',(67.5000000000091,-102.999999999958,-29.9999999999748));
#30815=CARTESIAN_POINT('',(67.5000000000102,-114.999999999957,-23.2499999999734));
#30816=CARTESIAN_POINT('Origin',(67.5000000000102,-114.999999999958,-29.9999999999734));
#30817=CARTESIAN_POINT('',(67.5000000000081,-90.9999999999569,-23.2499999999761));
#30818=CARTESIAN_POINT('',(67.5000000000091,-102.999999999957,-23.2499999999748));
#30819=CARTESIAN_POINT('Origin',(67.5000000000081,-90.9999999999577,-29.9999999999761));
#30820=CARTESIAN_POINT('Origin',(-94.9999999999911,-100.749999999987,-164.999999999975));
#30821=CARTESIAN_POINT('',(-94.9999999999913,-98.4999999999867,-158.371463208194));
#30822=CARTESIAN_POINT('',(-94.9999999999913,-98.4999999999882,-171.628536791757));
#30823=CARTESIAN_POINT('Origin',(-94.9999999999911,-100.749999999987,-164.999999999975));
#30824=CARTESIAN_POINT('',(-95.7125498784832,-93.7499999999875,-164.999999999976));
#30825=CARTESIAN_POINT('Origin',(-94.6624763733376,-100.749999999986,-164.999999999976));
#30826=CARTESIAN_POINT('',(-98.9999999999917,-93.7499999999878,-164.999999999976));
#30827=CARTESIAN_POINT('',(-94.9999999999917,-93.7499999999874,-164.999999999976));
#30828=CARTESIAN_POINT('Origin',(-98.9999999999911,-100.749999999988,-164.999999999975));
#30829=CARTESIAN_POINT('Origin',(-94.6624763733376,-100.749999999986,-164.999999999976));
#30830=CARTESIAN_POINT('Origin',(38.0550000000051,-57.556999999962,-44.99999999998));
#30831=CARTESIAN_POINT('',(51.7674904174255,-33.7196845774533,-42.4999999999827));
#30832=CARTESIAN_POINT('',(10.5673523229225,-56.7328488120256,-42.4999999999801));
#30833=CARTESIAN_POINT('Origin',(38.0550000000051,-57.5569999999617,-42.49999999998));
#30834=CARTESIAN_POINT('',(10.5550722920713,-57.620055994213,-47.49999999998));
#30835=CARTESIAN_POINT('Ctrl Pts',(10.5673523229226,-56.7328488120256,-42.4999999999801));
#30836=CARTESIAN_POINT('Ctrl Pts',(10.5584011171405,-57.0313954797058,-44.1797004210614));
#30837=CARTESIAN_POINT('Ctrl Pts',(10.5544011407209,-57.3273540261342,-45.8477046901759));
#30838=CARTESIAN_POINT('Ctrl Pts',(10.5550722920713,-57.620055994213,-47.49999999998));
#30839=CARTESIAN_POINT('',(52.5421582028762,-34.1823931111825,-47.4999999999826));
#30840=CARTESIAN_POINT('Origin',(38.0550000000051,-57.5569999999623,-47.49999999998));
#30841=CARTESIAN_POINT('Ctrl Pts',(52.542158202876,-34.1823931111825,-47.4999999999826));
#30842=CARTESIAN_POINT('Ctrl Pts',(52.2878704277616,-34.0247901514976,-45.8480650809791));
#30843=CARTESIAN_POINT('Ctrl Pts',(52.0293151832961,-33.8703000947384,-44.1791951589754));
#30844=CARTESIAN_POINT('Ctrl Pts',(51.7674904174254,-33.7196845774533,-42.4999999999827));
#30845=CARTESIAN_POINT('Origin',(-4.16333634234434E-12,49.0000000000344,
-47.4999999999922));
#30846=CARTESIAN_POINT('',(15.897355545321,-49.7282841269805,-6.99999999998086));
#30847=CARTESIAN_POINT('',(-10.2448885166815,-50.4738270062687,-6.99999999998077));
#30848=CARTESIAN_POINT('Origin',(-4.16333634234434E-12,49.0000000000391,
-6.99999999999224));
#30849=CARTESIAN_POINT('',(-7.28266813181056,-56.1260192332767,-37.4999999999801));
#30850=CARTESIAN_POINT('Ctrl Pts',(-10.2448885166816,-50.4738270062687,
-6.99999999998077));
#30851=CARTESIAN_POINT('Ctrl Pts',(-10.0507613055644,-50.7351013152882,
-8.36117250371065));
#30852=CARTESIAN_POINT('Ctrl Pts',(-9.86589792999223,-50.9968893519918,
-9.7347210061088));
#30853=CARTESIAN_POINT('Ctrl Pts',(-9.02371416128865,-52.2490441303325,
-16.3436456471985));
#30854=CARTESIAN_POINT('Ctrl Pts',(-8.47879759119335,-53.2442638527576,
-21.7106826495237));
#30855=CARTESIAN_POINT('Ctrl Pts',(-7.74223532726688,-54.8678382816299,
-30.5666815694324));
#30856=CARTESIAN_POINT('Ctrl Pts',(-7.49420517598333,-55.5012098316531,
-34.0479123391732));
#30857=CARTESIAN_POINT('Ctrl Pts',(-7.28266813181053,-56.1260192332767,
-37.4999999999801));
#30858=CARTESIAN_POINT('',(-5.67440940859151,-56.2250837624614,-37.4999999999801));
#30859=CARTESIAN_POINT('Origin',(-4.16333634234434E-12,49.0000000000356,
-37.4999999999922));
#30860=CARTESIAN_POINT('',(-5.20468772204855,-58.0147518663479,-47.4999999999799));
#30861=CARTESIAN_POINT('Ctrl Pts',(-5.67440940859151,-56.2250837624614,
-37.4999999999801));
#30862=CARTESIAN_POINT('Ctrl Pts',(-5.48790484690666,-56.8307083626227,
-40.8727282805478));
#30863=CARTESIAN_POINT('Ctrl Pts',(-5.33237987148615,-57.4289168050392,
-44.216665726727));
#30864=CARTESIAN_POINT('Ctrl Pts',(-5.20468772204851,-58.014751866348,-47.4999999999799));
#30865=CARTESIAN_POINT('Origin',(-4.16333634234434E-12,49.0000000000344,
-47.4999999999922));
#30866=CARTESIAN_POINT('',(14.5912051142114,-56.253033145551,-42.4999999999801));
#30867=CARTESIAN_POINT('Origin',(-4.16333634234434E-12,49.000000000035,
-42.4999999999922));
#30868=CARTESIAN_POINT('Ctrl Pts',(14.5912051142115,-56.253033145551,-42.4999999999801));
#30869=CARTESIAN_POINT('Ctrl Pts',(14.6413830074691,-55.3501238490315,-37.4669303649321));
#30870=CARTESIAN_POINT('Ctrl Pts',(14.7457120954502,-54.4208510744167,-32.3299558893149));
#30871=CARTESIAN_POINT('Ctrl Pts',(15.1306789058763,-52.2343060024871,-20.3730017764038));
#30872=CARTESIAN_POINT('Ctrl Pts',(15.4586955420126,-50.9698252107939,-13.5560974490108));
#30873=CARTESIAN_POINT('Ctrl Pts',(15.8973555453209,-49.7282841269806,-6.99999999998084));
#30874=CARTESIAN_POINT('Origin',(-26.6999999999944,-62.6999999999673,-42.4999999999794));
#30875=CARTESIAN_POINT('',(-42.5246458122939,-47.416656618518,-37.4999999999811));
#30876=CARTESIAN_POINT('Origin',(-26.6999999999944,-62.6999999999668,-37.4999999999794));
#30877=CARTESIAN_POINT('',(-43.7529288036085,-48.8004453589419,-47.499999999981));
#30878=CARTESIAN_POINT('Ctrl Pts',(-42.5246458122939,-47.416656618518,-37.4999999999811));
#30879=CARTESIAN_POINT('Ctrl Pts',(-42.9648697341177,-47.8724723040717,
-40.8727279978944));
#30880=CARTESIAN_POINT('Ctrl Pts',(-43.3741092094881,-48.3356834485934,
-44.216666118921));
#30881=CARTESIAN_POINT('Ctrl Pts',(-43.7529288036086,-48.8004453589419,
-47.499999999981));
#30882=CARTESIAN_POINT('Origin',(-26.6999999999944,-62.6999999999679,-47.4999999999794));
#30883=CARTESIAN_POINT('Origin',(-66.0000000000025,29.5000000000286,-47.49999999999));
#30884=CARTESIAN_POINT('',(-66.0000000000031,36.5000000000286,-47.4999999999908));
#30885=CARTESIAN_POINT('Origin',(-66.0000000000025,29.5000000000286,-47.49999999999));
#30886=CARTESIAN_POINT('',(-66.0000000000031,36.5000000000291,-43.4999999999908));
#30887=CARTESIAN_POINT('',(-66.0000000000031,36.5000000000286,-47.4999999999908));
#30888=CARTESIAN_POINT('Origin',(-66.0000000000025,29.5000000000292,-43.49999999999));
#30889=CARTESIAN_POINT('Origin',(88.4000000000047,-51.9999999999593,-60.4999999999806));
#30890=CARTESIAN_POINT('',(92.4000000000041,-44.999999999959,-60.4999999999814));
#30891=CARTESIAN_POINT('Origin',(92.4000000000047,-51.999999999959,-60.4999999999806));
#30892=CARTESIAN_POINT('',(84.4557280900048,-44.9999999999596,-60.4999999999814));
#30893=CARTESIAN_POINT('',(88.4000000000041,-44.9999999999593,-60.4999999999814));
#30894=CARTESIAN_POINT('',(85.0000000000041,-45.5697141142108,-57.7338793541052));
#30895=CARTESIAN_POINT('Ctrl Pts',(84.4557280900048,-44.9999999999596,-60.4999999999814));
#30896=CARTESIAN_POINT('Ctrl Pts',(84.4557280900048,-44.9999999999596,-59.8974676734178));
#30897=CARTESIAN_POINT('Ctrl Pts',(84.5285835749808,-45.0839151982962,-59.2517827630011));
#30898=CARTESIAN_POINT('Ctrl Pts',(84.7679545571492,-45.3368090946526,-58.3292893663764));
#30899=CARTESIAN_POINT('Ctrl Pts',(84.8741075050836,-45.4463147868548,-58.0207406499748));
#30900=CARTESIAN_POINT('Ctrl Pts',(85.000000000004,-45.5697141142107,-57.7338793541051));
#30901=CARTESIAN_POINT('',(85.0000000000047,-52.4302858857074,-53.5132372262401));
#30902=CARTESIAN_POINT('Origin',(85.0000000000047,-51.9999999999597,-60.4999999999806));
#30903=CARTESIAN_POINT('',(84.4000000000048,-53.0627460667651,-53.5811438230183));
#30904=CARTESIAN_POINT('Ctrl Pts',(85.0000000000047,-52.4302858857074,-53.5132372262401));
#30905=CARTESIAN_POINT('Ctrl Pts',(84.9277840037038,-52.5010717206654,-53.517596633691));
#30906=CARTESIAN_POINT('Ctrl Pts',(84.8566687357403,-52.5725688539638,-53.523079799516));
#30907=CARTESIAN_POINT('Ctrl Pts',(84.6572933790792,-52.7781017148926,-53.5420908204731));
#30908=CARTESIAN_POINT('Ctrl Pts',(84.5277608269389,-52.917878905895,-53.5588920227949));
#30909=CARTESIAN_POINT('Ctrl Pts',(84.4000000000048,-53.0627460667651,-53.5811438230183));
#30910=CARTESIAN_POINT('',(84.4000000000048,-53.0627460667667,-67.4188561769427));
#30911=CARTESIAN_POINT('Origin',(84.4000000000047,-51.9999999999597,-60.4999999999806));
#30912=CARTESIAN_POINT('',(85.0000000000047,-52.4302858857091,-67.486762773721));
#30913=CARTESIAN_POINT('Ctrl Pts',(84.4000000000048,-53.0627460667667,-67.4188561769427));
#30914=CARTESIAN_POINT('Ctrl Pts',(84.5277608269389,-52.9178789058966,-67.4411079771661));
#30915=CARTESIAN_POINT('Ctrl Pts',(84.6572933790792,-52.7781017148941,-67.4579091794879));
#30916=CARTESIAN_POINT('Ctrl Pts',(84.8566687357402,-52.5725688539654,-67.4769202004451));
#30917=CARTESIAN_POINT('Ctrl Pts',(84.9277840037038,-52.501071720667,-67.4824033662701));
#30918=CARTESIAN_POINT('Ctrl Pts',(85.0000000000047,-52.4302858857091,-67.486762773721));
#30919=CARTESIAN_POINT('',(85.0000000000041,-45.5697141142114,-63.2661206458575));
#30920=CARTESIAN_POINT('Origin',(85.0000000000047,-51.9999999999597,-60.4999999999806));
#30921=CARTESIAN_POINT('Ctrl Pts',(85.000000000004,-45.5697141142114,-63.2661206458576));
#30922=CARTESIAN_POINT('Ctrl Pts',(84.8741075050836,-45.4463147868554,-62.9792593499879));
#30923=CARTESIAN_POINT('Ctrl Pts',(84.7679545571492,-45.3368090946531,-62.6707106335864));
#30924=CARTESIAN_POINT('Ctrl Pts',(84.5285835749809,-45.0839151982965,-61.7482172369618));
#30925=CARTESIAN_POINT('Ctrl Pts',(84.4557280900048,-44.9999999999597,-61.102532326545));
#30926=CARTESIAN_POINT('Ctrl Pts',(84.4557280900048,-44.9999999999597,-60.4999999999814));
#30927=CARTESIAN_POINT('Origin',(-88.4,2.21092675417589E-11,-87.4999999999866));
#30928=CARTESIAN_POINT('',(-85.,2.32194905663841E-11,-80.4999999999866));
#30929=CARTESIAN_POINT('',(-85.,2.16096671806776E-11,-94.4999999999866));
#30930=CARTESIAN_POINT('Origin',(-85.,2.24145788735308E-11,-87.4999999999866));
#30931=CARTESIAN_POINT('',(-84.4,4.46250000002306,-82.1068475128048));
#30932=CARTESIAN_POINT('Origin',(-84.9999999999962,3.66340291435563E-11,
-87.4999999999461));
#30933=CARTESIAN_POINT('',(-84.4000000000002,7.00000000002246,-87.4999999999874));
#30934=CARTESIAN_POINT('Origin',(-84.4,2.24700900247621E-11,-87.4999999999866));
#30935=CARTESIAN_POINT('',(-92.4000000000006,7.00000000002176,-87.4999999999874));
#30936=CARTESIAN_POINT('',(-88.4000000000006,7.00000000002211,-87.4999999999874));
#30937=CARTESIAN_POINT('Origin',(-92.4,2.17484450587558E-11,-87.4999999999866));
#30938=CARTESIAN_POINT('',(-84.4,4.46250000002184,-92.8931524871694));
#30939=CARTESIAN_POINT('Origin',(-84.4,2.24700900247621E-11,-87.4999999999866));
#30940=CARTESIAN_POINT('Origin',(-84.9999999999965,2.80445537735029E-11,
-87.4999999999995));
#30941=CARTESIAN_POINT('Origin',(1.11022302462516E-12,-11.1689999999808,
-179.499999999986));
#30942=CARTESIAN_POINT('',(-5.86106217982448E-12,68.8310000000173,-196.499999999995));
#30943=CARTESIAN_POINT('Origin',(1.11022302462516E-12,-11.1689999999827,
-196.499999999986));
#30944=CARTESIAN_POINT('',(-5.86106217982472E-12,68.8310000000201,-172.499999999995));
#30945=CARTESIAN_POINT('',(-5.86106217982465E-12,68.8310000000192,-179.499999999995));
#30946=CARTESIAN_POINT('Origin',(1.11022302462516E-12,-11.16899999998,-172.499999999986));
#30947=CARTESIAN_POINT('Origin',(1.11022302462516E-13,3.92899688478332E-11,
-5.2499999999866));
#30948=CARTESIAN_POINT('',(-3.37462029976237E-12,40.0000000000391,-6.99999999999121));
#30949=CARTESIAN_POINT('Origin',(1.11022302462516E-13,3.90956798185238E-11,
-6.9999999999866));
#30950=CARTESIAN_POINT('',(-3.3746202997624E-12,40.0000000000395,-3.4999999999912));
#30951=CARTESIAN_POINT('',(-3.37462029976239E-12,40.0000000000393,-5.24999999999121));
#30952=CARTESIAN_POINT('Origin',(1.11022302462516E-13,3.94842578771426E-11,
-3.4999999999866));
#30953=CARTESIAN_POINT('Origin',(-45.0000000000069,80.7485954613074,-137.259999999996));
#30954=CARTESIAN_POINT('',(-40.5000000000059,69.6242977306741,-50.1388507296581));
#30955=CARTESIAN_POINT('',(-49.500000000006,69.6242977306733,-50.1388507296581));
#30956=CARTESIAN_POINT('Ctrl Pts',(-49.5000000000044,69.6242977306726,-50.1388507296569));
#30957=CARTESIAN_POINT('Ctrl Pts',(-49.4390982354682,69.5996617539082,-50.0984034235873));
#30958=CARTESIAN_POINT('Ctrl Pts',(-49.3768762455399,69.5750761416804,-50.0591199168394));
#30959=CARTESIAN_POINT('Ctrl Pts',(-49.0593786189297,69.4527670848549,-49.8683860724675));
#30960=CARTESIAN_POINT('Ctrl Pts',(-48.7892136307126,69.3594387044218,-49.7382482521322));
#30961=CARTESIAN_POINT('Ctrl Pts',(-48.0207556703975,69.122587413154,-49.4258938436431));
#30962=CARTESIAN_POINT('Ctrl Pts',(-47.4278637439859,68.980519656034,-49.2670353254958));
#30963=CARTESIAN_POINT('Ctrl Pts',(-46.2057776234041,68.7933356998361,-49.066423146127));
#30964=CARTESIAN_POINT('Ctrl Pts',(-45.5767473719908,68.7485954613172,-49.0233224566437));
#30965=CARTESIAN_POINT('Ctrl Pts',(-44.423252628021,68.7485954613173,-49.0233224566437));
#30966=CARTESIAN_POINT('Ctrl Pts',(-43.7942223766076,68.7933356998363,-49.066423146127));
#30967=CARTESIAN_POINT('Ctrl Pts',(-42.5721362560258,68.9805196560344,-49.2670353254958));
#30968=CARTESIAN_POINT('Ctrl Pts',(-41.9792443296143,69.1225874131545,-49.4258938436431));
#30969=CARTESIAN_POINT('Ctrl Pts',(-41.2107863692992,69.3594387044225,-49.7382482521322));
#30970=CARTESIAN_POINT('Ctrl Pts',(-40.9406213810821,69.4527670848557,-49.8683860724675));
#30971=CARTESIAN_POINT('Ctrl Pts',(-40.6231237544707,69.5750761416816,-50.0591199168402));
#30972=CARTESIAN_POINT('Ctrl Pts',(-40.5609017645412,69.59966175391,-50.0984034235889));
#30973=CARTESIAN_POINT('Ctrl Pts',(-40.5000000000039,69.6242977306749,-50.1388507296593));
#30974=CARTESIAN_POINT('',(-40.5000000000059,69.6242977306647,-134.381149270331));
#30975=CARTESIAN_POINT('',(-40.5000000000059,69.6242977306643,-137.259999999995));
#30976=CARTESIAN_POINT('',(-49.500000000006,69.6242977306639,-134.381149270331));
#30977=CARTESIAN_POINT('Ctrl Pts',(-40.5000000000075,69.624297730664,-134.381149270332));
#30978=CARTESIAN_POINT('Ctrl Pts',(-40.5609017645436,69.5996617538996,-134.421596576402));
#30979=CARTESIAN_POINT('Ctrl Pts',(-40.623123754472,69.5750761416717,-134.46088008315));
#30980=CARTESIAN_POINT('Ctrl Pts',(-40.9406213810821,69.4527670848462,-134.651613927522));
#30981=CARTESIAN_POINT('Ctrl Pts',(-41.2107863692992,69.359438704413,-134.781751747857));
#30982=CARTESIAN_POINT('Ctrl Pts',(-41.9792443296143,69.1225874131449,-135.094106156346));
#30983=CARTESIAN_POINT('Ctrl Pts',(-42.5721362560258,68.9805196560248,-135.252964674493));
#30984=CARTESIAN_POINT('Ctrl Pts',(-43.7942223766076,68.7933356998266,-135.453576853862));
#30985=CARTESIAN_POINT('Ctrl Pts',(-44.4232526280209,68.7485954613077,-135.496677543345));
#30986=CARTESIAN_POINT('Ctrl Pts',(-45.5767473719907,68.7485954613076,-135.496677543345));
#30987=CARTESIAN_POINT('Ctrl Pts',(-46.2057776234041,68.7933356998264,-135.453576853862));
#30988=CARTESIAN_POINT('Ctrl Pts',(-47.4278637439859,68.9805196560244,-135.252964674493));
#30989=CARTESIAN_POINT('Ctrl Pts',(-48.0207556703975,69.1225874131444,-135.094106156346));
#30990=CARTESIAN_POINT('Ctrl Pts',(-48.7892136307126,69.3594387044123,-134.781751747857));
#30991=CARTESIAN_POINT('Ctrl Pts',(-49.0593786189297,69.4527670848454,-134.651613927522));
#30992=CARTESIAN_POINT('Ctrl Pts',(-49.3768762455412,69.5750761416714,-134.460880083149));
#30993=CARTESIAN_POINT('Ctrl Pts',(-49.4390982354707,69.5996617538998,-134.4215965764));
#30994=CARTESIAN_POINT('Ctrl Pts',(-49.5000000000081,69.6242977306647,-134.38114927033));
#30995=CARTESIAN_POINT('',(-49.500000000006,69.6242977306636,-137.259999999995));
#30996=CARTESIAN_POINT('Origin',(-27.000000000007,80.748595461309,-137.259999999996));
#30997=CARTESIAN_POINT('',(-22.500000000006,69.6242977306757,-50.1388507296581));
#30998=CARTESIAN_POINT('',(-31.500000000006,69.6242977306749,-50.1388507296581));
#30999=CARTESIAN_POINT('Ctrl Pts',(-31.5000000000043,69.6242977306742,-50.1388507296569));
#31000=CARTESIAN_POINT('Ctrl Pts',(-31.4390982354682,69.5996617539098,-50.0984034235873));
#31001=CARTESIAN_POINT('Ctrl Pts',(-31.3768762455399,69.5750761416819,-50.0591199168394));
#31002=CARTESIAN_POINT('Ctrl Pts',(-31.0593786189298,69.4527670848565,-49.8683860724675));
#31003=CARTESIAN_POINT('Ctrl Pts',(-30.7892136307126,69.3594387044234,-49.7382482521322));
#31004=CARTESIAN_POINT('Ctrl Pts',(-30.0207556703975,69.1225874131556,-49.4258938436431));
#31005=CARTESIAN_POINT('Ctrl Pts',(-29.4278637439859,68.9805196560356,-49.2670353254958));
#31006=CARTESIAN_POINT('Ctrl Pts',(-28.2057776234042,68.7933356998377,-49.066423146127));
#31007=CARTESIAN_POINT('Ctrl Pts',(-27.5767473719908,68.7485954613188,-49.0233224566438));
#31008=CARTESIAN_POINT('Ctrl Pts',(-26.423252628021,68.7485954613189,-49.0233224566438));
#31009=CARTESIAN_POINT('Ctrl Pts',(-25.7942223766076,68.7933356998379,-49.066423146127));
#31010=CARTESIAN_POINT('Ctrl Pts',(-24.5721362560259,68.980519656036,-49.2670353254958));
#31011=CARTESIAN_POINT('Ctrl Pts',(-23.9792443296144,69.1225874131561,-49.4258938436431));
#31012=CARTESIAN_POINT('Ctrl Pts',(-23.2107863692993,69.3594387044241,-49.7382482521322));
#31013=CARTESIAN_POINT('Ctrl Pts',(-22.9406213810822,69.4527670848572,-49.8683860724675));
#31014=CARTESIAN_POINT('Ctrl Pts',(-22.6231237544708,69.5750761416832,-50.0591199168402));
#31015=CARTESIAN_POINT('Ctrl Pts',(-22.5609017645412,69.5996617539116,-50.0984034235889));
#31016=CARTESIAN_POINT('Ctrl Pts',(-22.5000000000039,69.6242977306765,-50.1388507296593));
#31017=CARTESIAN_POINT('',(-22.500000000006,69.6242977306663,-134.381149270331));
#31018=CARTESIAN_POINT('',(-22.500000000006,69.6242977306659,-137.259999999995));
#31019=CARTESIAN_POINT('',(-31.500000000006,69.6242977306654,-134.381149270331));
#31020=CARTESIAN_POINT('Ctrl Pts',(-22.5000000000075,69.6242977306656,-134.381149270332));
#31021=CARTESIAN_POINT('Ctrl Pts',(-22.5609017645437,69.5996617539012,-134.421596576402));
#31022=CARTESIAN_POINT('Ctrl Pts',(-22.623123754472,69.5750761416733,-134.46088008315));
#31023=CARTESIAN_POINT('Ctrl Pts',(-22.9406213810822,69.4527670848478,-134.651613927522));
#31024=CARTESIAN_POINT('Ctrl Pts',(-23.2107863692993,69.3594387044146,-134.781751747857));
#31025=CARTESIAN_POINT('Ctrl Pts',(-23.9792443296144,69.1225874131465,-135.094106156346));
#31026=CARTESIAN_POINT('Ctrl Pts',(-24.5721362560259,68.9805196560264,-135.252964674493));
#31027=CARTESIAN_POINT('Ctrl Pts',(-25.7942223766076,68.7933356998282,-135.453576853862));
#31028=CARTESIAN_POINT('Ctrl Pts',(-26.423252628021,68.7485954613093,-135.496677543345));
#31029=CARTESIAN_POINT('Ctrl Pts',(-27.5767473719908,68.7485954613092,-135.496677543345));
#31030=CARTESIAN_POINT('Ctrl Pts',(-28.2057776234042,68.793335699828,-135.453576853862));
#31031=CARTESIAN_POINT('Ctrl Pts',(-29.4278637439859,68.980519656026,-135.252964674493));
#31032=CARTESIAN_POINT('Ctrl Pts',(-30.0207556703975,69.122587413146,-135.094106156346));
#31033=CARTESIAN_POINT('Ctrl Pts',(-30.7892136307126,69.3594387044139,-134.781751747857));
#31034=CARTESIAN_POINT('Ctrl Pts',(-31.0593786189298,69.4527670848471,-134.651613927522));
#31035=CARTESIAN_POINT('Ctrl Pts',(-31.3768762455412,69.575076141673,-134.460880083149));
#31036=CARTESIAN_POINT('Ctrl Pts',(-31.4390982354707,69.5996617539014,-134.4215965764));
#31037=CARTESIAN_POINT('Ctrl Pts',(-31.500000000008,69.6242977306663,-134.38114927033));
#31038=CARTESIAN_POINT('',(-31.500000000006,69.6242977306651,-137.259999999995));
#31039=CARTESIAN_POINT('Origin',(-9.00000000000695,80.7485954613106,-137.259999999996));
#31040=CARTESIAN_POINT('',(-6.66025403785028,68.9789060502699,-58.2599999999945));
#31041=CARTESIAN_POINT('',(-11.7870568576517,69.0767355378866,-49.3801170357112));
#31042=CARTESIAN_POINT('Origin',(-9.00000000010824,80.7485954607085,-54.2074411165631));
#31043=CARTESIAN_POINT('',(-4.50000000000594,69.624297730676,-60.85934207678));
#31044=CARTESIAN_POINT('Ctrl Pts',(-4.50000000000591,69.6242977306761,-60.85934207678));
#31045=CARTESIAN_POINT('Ctrl Pts',(-4.57072744769444,69.5956870693737,-60.798846259467));
#31046=CARTESIAN_POINT('Ctrl Pts',(-4.6401768168913,69.5683786357621,-60.7377313283798));
#31047=CARTESIAN_POINT('Ctrl Pts',(-5.44240225889553,69.2611409903921,-60.0120911133602));
#31048=CARTESIAN_POINT('Ctrl Pts',(-6.12426404754931,69.085457750299,-59.1883618955442));
#31049=CARTESIAN_POINT('Ctrl Pts',(-6.66025403785028,68.9789060502699,-58.2599999999945));
#31050=CARTESIAN_POINT('',(-4.50000000000611,69.6242977306689,-123.660657923209));
#31051=CARTESIAN_POINT('',(-4.50000000000594,69.6242977306675,-137.259999999995));
#31052=CARTESIAN_POINT('',(-6.66025403785028,68.9789060502623,-126.259999999995));
#31053=CARTESIAN_POINT('Ctrl Pts',(-6.66025403785036,68.9789060502623,-126.259999999995));
#31054=CARTESIAN_POINT('Ctrl Pts',(-6.12426404754937,69.0854577502916,-125.331638104445));
#31055=CARTESIAN_POINT('Ctrl Pts',(-5.44240225889557,69.2611409903848,-124.507908886629));
#31056=CARTESIAN_POINT('Ctrl Pts',(-4.64017681689139,69.568378635755,-123.782268671609));
#31057=CARTESIAN_POINT('Ctrl Pts',(-4.57072744769462,69.5956870693666,-123.721153740522));
#31058=CARTESIAN_POINT('Ctrl Pts',(-4.50000000000619,69.6242977306689,-123.660657923209));
#31059=CARTESIAN_POINT('',(-11.7870568576531,69.0767355378777,-135.13988296428));
#31060=CARTESIAN_POINT('Origin',(-9.00000000026207,80.7485954590947,-130.312558883691));
#31061=CARTESIAN_POINT('',(-13.5000000000061,69.6242977306671,-134.381149270331));
#31062=CARTESIAN_POINT('Ctrl Pts',(-13.5000000000062,69.6242977306671,-134.381149270331));
#31063=CARTESIAN_POINT('Ctrl Pts',(-13.4390982354695,69.5996617539025,-134.421596576401));
#31064=CARTESIAN_POINT('Ctrl Pts',(-13.3768762455405,69.5750761416743,-134.460880083149));
#31065=CARTESIAN_POINT('Ctrl Pts',(-13.0593786189297,69.4527670848486,-134.651613927522));
#31066=CARTESIAN_POINT('Ctrl Pts',(-12.7892136307126,69.3594387044155,-134.781751747857));
#31067=CARTESIAN_POINT('Ctrl Pts',(-12.2998487382835,69.2086084538895,-134.980663450779));
#31068=CARTESIAN_POINT('Ctrl Pts',(-12.0489093664513,69.13926180491,-135.066126567241));
#31069=CARTESIAN_POINT('Ctrl Pts',(-11.7870568576528,69.0767355378775,-135.139882964279));
#31070=CARTESIAN_POINT('',(-13.5000000000059,69.6242977306765,-50.1388507296581));
#31071=CARTESIAN_POINT('',(-13.5000000000059,69.6242977306667,-137.259999999995));
#31072=CARTESIAN_POINT('Ctrl Pts',(-11.787056857652,69.0767355378869,-49.3801170357097));
#31073=CARTESIAN_POINT('Ctrl Pts',(-12.0489093664508,69.1392618049194,-49.4538734327484));
#31074=CARTESIAN_POINT('Ctrl Pts',(-12.2998487382833,69.208608453899,-49.5393365492105));
#31075=CARTESIAN_POINT('Ctrl Pts',(-12.7892136307126,69.359438704425,-49.7382482521323));
#31076=CARTESIAN_POINT('Ctrl Pts',(-13.0593786189297,69.4527670848581,-49.8683860724675));
#31077=CARTESIAN_POINT('Ctrl Pts',(-13.3768762455404,69.5750761416838,-50.0591199168398));
#31078=CARTESIAN_POINT('Ctrl Pts',(-13.4390982354693,69.5996617539118,-50.0984034235881));
#31079=CARTESIAN_POINT('Ctrl Pts',(-13.500000000006,69.6242977306765,-50.138850729658));
#31080=CARTESIAN_POINT('Origin',(26.9999999999931,80.7485954613137,-137.259999999996));
#31081=CARTESIAN_POINT('',(31.499999999994,69.6242977306804,-50.1388507296581));
#31082=CARTESIAN_POINT('',(22.4999999999941,69.6242977306796,-50.1388507296581));
#31083=CARTESIAN_POINT('Ctrl Pts',(22.4999999999957,69.6242977306789,-50.1388507296569));
#31084=CARTESIAN_POINT('Ctrl Pts',(22.5609017645318,69.5996617539145,-50.0984034235874));
#31085=CARTESIAN_POINT('Ctrl Pts',(22.6231237544602,69.5750761416866,-50.0591199168394));
#31086=CARTESIAN_POINT('Ctrl Pts',(22.9406213810703,69.4527670848612,-49.8683860724675));
#31087=CARTESIAN_POINT('Ctrl Pts',(23.2107863692874,69.3594387044281,-49.7382482521322));
#31088=CARTESIAN_POINT('Ctrl Pts',(23.9792443296025,69.1225874131603,-49.4258938436431));
#31089=CARTESIAN_POINT('Ctrl Pts',(24.5721362560141,68.9805196560403,-49.2670353254958));
#31090=CARTESIAN_POINT('Ctrl Pts',(25.7942223765959,68.7933356998424,-49.066423146127));
#31091=CARTESIAN_POINT('Ctrl Pts',(26.4232526280092,68.7485954613235,-49.0233224566437));
#31092=CARTESIAN_POINT('Ctrl Pts',(27.5767473719791,68.7485954613236,-49.0233224566437));
#31093=CARTESIAN_POINT('Ctrl Pts',(28.2057776233924,68.7933356998426,-49.066423146127));
#31094=CARTESIAN_POINT('Ctrl Pts',(29.4278637439741,68.9805196560407,-49.2670353254958));
#31095=CARTESIAN_POINT('Ctrl Pts',(30.0207556703857,69.1225874131608,-49.4258938436431));
#31096=CARTESIAN_POINT('Ctrl Pts',(30.7892136307008,69.3594387044288,-49.7382482521322));
#31097=CARTESIAN_POINT('Ctrl Pts',(31.0593786189179,69.4527670848619,-49.8683860724675));
#31098=CARTESIAN_POINT('Ctrl Pts',(31.3768762455292,69.5750761416879,-50.0591199168402));
#31099=CARTESIAN_POINT('Ctrl Pts',(31.4390982354588,69.5996617539163,-50.0984034235889));
#31100=CARTESIAN_POINT('Ctrl Pts',(31.4999999999961,69.6242977306811,-50.1388507296593));
#31101=CARTESIAN_POINT('',(31.499999999994,69.6242977306789,-63.2599999999946));
#31102=CARTESIAN_POINT('',(31.499999999994,69.6242977306707,-137.259999999995));
#31103=CARTESIAN_POINT('',(22.4999999999941,69.6242977306781,-63.2599999999946));
#31104=CARTESIAN_POINT('Origin',(26.9999999999931,80.748595461322,-63.2599999999959));
#31105=CARTESIAN_POINT('',(22.4999999999941,69.6242977306698,-137.259999999995));
#31106=CARTESIAN_POINT('Origin',(44.9999999999931,80.7485954613153,-137.259999999996));
#31107=CARTESIAN_POINT('',(49.4999999999941,69.624297730682,-50.1388507296581));
#31108=CARTESIAN_POINT('',(40.499999999994,69.6242977306812,-50.1388507296581));
#31109=CARTESIAN_POINT('Ctrl Pts',(40.4999999999957,69.6242977306805,-50.1388507296569));
#31110=CARTESIAN_POINT('Ctrl Pts',(40.5609017645319,69.5996617539161,-50.0984034235874));
#31111=CARTESIAN_POINT('Ctrl Pts',(40.6231237544602,69.5750761416882,-50.0591199168395));
#31112=CARTESIAN_POINT('Ctrl Pts',(40.9406213810703,69.4527670848628,-49.8683860724675));
#31113=CARTESIAN_POINT('Ctrl Pts',(41.2107863692875,69.3594387044297,-49.7382482521323));
#31114=CARTESIAN_POINT('Ctrl Pts',(41.9792443296026,69.1225874131619,-49.4258938436431));
#31115=CARTESIAN_POINT('Ctrl Pts',(42.5721362560142,68.9805196560419,-49.2670353254958));
#31116=CARTESIAN_POINT('Ctrl Pts',(43.7942223765959,68.793335699844,-49.0664231461271));
#31117=CARTESIAN_POINT('Ctrl Pts',(44.4232526280093,68.7485954613251,-49.0233224566438));
#31118=CARTESIAN_POINT('Ctrl Pts',(45.5767473719791,68.7485954613252,-49.0233224566438));
#31119=CARTESIAN_POINT('Ctrl Pts',(46.2057776233924,68.7933356998442,-49.0664231461271));
#31120=CARTESIAN_POINT('Ctrl Pts',(47.4278637439741,68.9805196560423,-49.2670353254959));
#31121=CARTESIAN_POINT('Ctrl Pts',(48.0207556703856,69.1225874131624,-49.4258938436432));
#31122=CARTESIAN_POINT('Ctrl Pts',(48.7892136307007,69.3594387044304,-49.7382482521323));
#31123=CARTESIAN_POINT('Ctrl Pts',(49.0593786189178,69.4527670848635,-49.8683860724676));
#31124=CARTESIAN_POINT('Ctrl Pts',(49.3768762455292,69.5750761416895,-50.0591199168403));
#31125=CARTESIAN_POINT('Ctrl Pts',(49.4390982354588,69.5996617539179,-50.098403423589));
#31126=CARTESIAN_POINT('Ctrl Pts',(49.4999999999961,69.6242977306828,-50.1388507296594));
#31127=CARTESIAN_POINT('',(49.4999999999941,69.6242977306725,-134.381149270331));
#31128=CARTESIAN_POINT('',(49.4999999999941,69.6242977306722,-137.259999999995));
#31129=CARTESIAN_POINT('',(40.499999999994,69.6242977306718,-134.381149270331));
#31130=CARTESIAN_POINT('Ctrl Pts',(49.4999999999925,69.6242977306719,-134.381149270332));
#31131=CARTESIAN_POINT('Ctrl Pts',(49.4390982354563,69.5996617539075,-134.421596576402));
#31132=CARTESIAN_POINT('Ctrl Pts',(49.376876245528,69.5750761416795,-134.46088008315));
#31133=CARTESIAN_POINT('Ctrl Pts',(49.0593786189179,69.452767084854,-134.651613927522));
#31134=CARTESIAN_POINT('Ctrl Pts',(48.7892136307007,69.3594387044209,-134.781751747857));
#31135=CARTESIAN_POINT('Ctrl Pts',(48.0207556703856,69.1225874131528,-135.094106156346));
#31136=CARTESIAN_POINT('Ctrl Pts',(47.4278637439741,68.9805196560327,-135.252964674493));
#31137=CARTESIAN_POINT('Ctrl Pts',(46.2057776233924,68.7933356998346,-135.453576853862));
#31138=CARTESIAN_POINT('Ctrl Pts',(45.576747371979,68.7485954613156,-135.496677543345));
#31139=CARTESIAN_POINT('Ctrl Pts',(44.4232526280092,68.7485954613155,-135.496677543345));
#31140=CARTESIAN_POINT('Ctrl Pts',(43.7942223765959,68.7933356998343,-135.453576853862));
#31141=CARTESIAN_POINT('Ctrl Pts',(42.5721362560142,68.9805196560323,-135.252964674493));
#31142=CARTESIAN_POINT('Ctrl Pts',(41.9792443296026,69.1225874131523,-135.094106156346));
#31143=CARTESIAN_POINT('Ctrl Pts',(41.2107863692875,69.3594387044202,-134.781751747857));
#31144=CARTESIAN_POINT('Ctrl Pts',(40.9406213810703,69.4527670848533,-134.651613927522));
#31145=CARTESIAN_POINT('Ctrl Pts',(40.6231237544589,69.5750761416793,-134.460880083149));
#31146=CARTESIAN_POINT('Ctrl Pts',(40.5609017645293,69.5996617539077,-134.4215965764));
#31147=CARTESIAN_POINT('Ctrl Pts',(40.499999999992,69.6242977306726,-134.38114927033));
#31148=CARTESIAN_POINT('',(40.499999999994,69.6242977306714,-137.259999999995));
#31149=CARTESIAN_POINT('Origin',(1.11022302462516E-12,-11.1689999999816,
-186.499999999986));
#31150=CARTESIAN_POINT('',(-44.8103167727357,-39.4715707441228,-208.140791933168));
#31151=CARTESIAN_POINT('',(52.999999999995,-11.1689999999795,-208.140791933169));
#31152=CARTESIAN_POINT('Origin',(1.11022302462516E-12,-11.1689999999841,
-208.140791933171));
#31153=CARTESIAN_POINT('',(-51.6986185553089,-22.8417391589202,-208.140791933169));
#31154=CARTESIAN_POINT('Origin',(1.11022302462516E-12,-11.1689999999841,
-208.140791933171));
#31155=CARTESIAN_POINT('',(-51.6986185553089,-22.8417391589189,-196.499999999984));
#31156=CARTESIAN_POINT('',(-51.6986185553089,-22.8417391589189,-196.399999999984));
#31157=CARTESIAN_POINT('',(-44.8103167727357,-39.4715707441215,-196.499999999982));
#31158=CARTESIAN_POINT('Origin',(1.11022302462516E-12,-11.1689999999827,
-196.499999999986));
#31159=CARTESIAN_POINT('',(-44.8103167727357,-39.4715707441215,-196.399999999982));
#31160=CARTESIAN_POINT('Origin',(6.07847105982273E-12,-76.1689999999842,
-209.227922061336));
#31161=CARTESIAN_POINT('',(6.47170803469214E-12,-80.6689999999827,-196.499999999977));
#31162=CARTESIAN_POINT('Origin',(6.07847105982273E-12,-76.1689999999827,
-196.499999999978));
#31163=CARTESIAN_POINT('',(6.47170803469204E-12,-80.6689999999816,-186.499999999977));
#31164=CARTESIAN_POINT('',(6.47170803469227E-12,-80.6689999999842,-209.227922061336));
#31165=CARTESIAN_POINT('Origin',(6.07847105982273E-12,-76.1689999999816,
-186.499999999978));
#31166=CARTESIAN_POINT('Origin',(65.0000000000011,-11.168999999979,-209.227922061344));
#31167=CARTESIAN_POINT('',(65.0000000000015,-15.6689999999776,-196.499999999985));
#31168=CARTESIAN_POINT('Origin',(65.0000000000011,-11.1689999999776,-196.499999999986));
#31169=CARTESIAN_POINT('',(65.0000000000015,-15.6689999999764,-186.499999999985));
#31170=CARTESIAN_POINT('',(65.0000000000015,-15.668999999979,-209.227922061343));
#31171=CARTESIAN_POINT('Origin',(65.0000000000011,-11.1689999999764,-186.499999999986));
#31172=CARTESIAN_POINT('Origin',(-4.35762537165374E-12,53.8310000000158,
-209.227922061351));
#31173=CARTESIAN_POINT('',(-3.96438839678434E-12,49.3310000000173,-196.499999999992));
#31174=CARTESIAN_POINT('Origin',(-4.35762537165374E-12,53.8310000000173,
-196.499999999993));
#31175=CARTESIAN_POINT('',(-3.96438839678444E-12,49.3310000000184,-186.499999999992));
#31176=CARTESIAN_POINT('',(-3.96438839678421E-12,49.3310000000158,-209.227922061351));
#31177=CARTESIAN_POINT('Origin',(-4.35762537165374E-12,53.8310000000184,
-186.499999999993));
#31178=CARTESIAN_POINT('Origin',(-64.9999999999989,-11.1689999999899,-209.227922061344));
#31179=CARTESIAN_POINT('',(-64.9999999999985,-15.6689999999884,-196.499999999985));
#31180=CARTESIAN_POINT('Origin',(-64.9999999999989,-11.1689999999884,-196.499999999986));
#31181=CARTESIAN_POINT('',(-64.9999999999985,-15.6689999999872,-186.499999999985));
#31182=CARTESIAN_POINT('',(-64.9999999999985,-15.6689999999899,-209.227922061343));
#31183=CARTESIAN_POINT('Origin',(-64.9999999999989,-11.1689999999873,-186.499999999986));
#31184=CARTESIAN_POINT('Origin',(1.11022302462516E-13,3.97063024820676E-11,
-1.7499999999866));
#31185=CARTESIAN_POINT('',(-1.63179899864992E-12,20.0000000000395,-3.4999999999889));
#31186=CARTESIAN_POINT('Origin',(1.11022302462516E-13,3.94842578771426E-11,
-3.4999999999866));
#31187=CARTESIAN_POINT('',(-1.63179899864995E-12,20.0000000000399,1.11022302462516E-11));
#31188=CARTESIAN_POINT('',(-1.63179899864994E-12,20.0000000000397,-1.7499999999889));
#31189=CARTESIAN_POINT('Origin',(1.11022302462516E-13,3.99005915113771E-11,
1.34059430223488E-11));
#31190=CARTESIAN_POINT('Origin',(26.9999999999931,80.7485954613137,-137.259999999996));
#31191=CARTESIAN_POINT('',(31.499999999994,69.6242977306724,-121.259999999995));
#31192=CARTESIAN_POINT('',(22.4999999999941,69.6242977306716,-121.259999999995));
#31193=CARTESIAN_POINT('Origin',(26.9999999999931,80.7485954613155,-121.259999999996));
#31194=CARTESIAN_POINT('',(31.499999999994,69.624297730671,-134.381149270331));
#31195=CARTESIAN_POINT('',(31.499999999994,69.6242977306707,-137.259999999995));
#31196=CARTESIAN_POINT('',(22.4999999999941,69.6242977306702,-134.381149270331));
#31197=CARTESIAN_POINT('Ctrl Pts',(31.4999999999925,69.6242977306703,-134.381149270332));
#31198=CARTESIAN_POINT('Ctrl Pts',(31.4390982354563,69.5996617539059,-134.421596576402));
#31199=CARTESIAN_POINT('Ctrl Pts',(31.376876245528,69.575076141678,-134.46088008315));
#31200=CARTESIAN_POINT('Ctrl Pts',(31.0593786189179,69.4527670848525,-134.651613927522));
#31201=CARTESIAN_POINT('Ctrl Pts',(30.7892136307008,69.3594387044192,-134.781751747857));
#31202=CARTESIAN_POINT('Ctrl Pts',(30.0207556703857,69.1225874131512,-135.094106156346));
#31203=CARTESIAN_POINT('Ctrl Pts',(29.4278637439741,68.9805196560311,-135.252964674493));
#31204=CARTESIAN_POINT('Ctrl Pts',(28.2057776233924,68.7933356998329,-135.453576853862));
#31205=CARTESIAN_POINT('Ctrl Pts',(27.576747371979,68.748595461314,-135.496677543345));
#31206=CARTESIAN_POINT('Ctrl Pts',(26.4232526280092,68.7485954613139,-135.496677543345));
#31207=CARTESIAN_POINT('Ctrl Pts',(25.7942223765959,68.7933356998327,-135.453576853862));
#31208=CARTESIAN_POINT('Ctrl Pts',(24.5721362560141,68.9805196560307,-135.252964674493));
#31209=CARTESIAN_POINT('Ctrl Pts',(23.9792443296025,69.1225874131507,-135.094106156346));
#31210=CARTESIAN_POINT('Ctrl Pts',(23.2107863692874,69.3594387044186,-134.781751747857));
#31211=CARTESIAN_POINT('Ctrl Pts',(22.9406213810703,69.4527670848518,-134.651613927522));
#31212=CARTESIAN_POINT('Ctrl Pts',(22.6231237544589,69.5750761416777,-134.460880083149));
#31213=CARTESIAN_POINT('Ctrl Pts',(22.5609017645293,69.5996617539061,-134.4215965764));
#31214=CARTESIAN_POINT('Ctrl Pts',(22.499999999992,69.624297730671,-134.38114927033));
#31215=CARTESIAN_POINT('',(22.4999999999941,69.6242977306698,-137.259999999995));
#31216=CARTESIAN_POINT('Origin',(1.99999999999398,70.5000000000341,-53.2599999999947));
#31217=CARTESIAN_POINT('',(10.6602540378387,66.5000000000341,-58.2599999999942));
#31218=CARTESIAN_POINT('',(-6.66025403785006,66.5000000000326,-58.2599999999943));
#31219=CARTESIAN_POINT('Origin',(1.99999999999431,66.5000000000339,-53.2599999999943));
#31220=CARTESIAN_POINT('',(10.6602540378385,68.8640022192357,-58.2599999999945));
#31221=CARTESIAN_POINT('',(10.6602540378383,70.5000000000341,-58.2599999999947));
#31222=CARTESIAN_POINT('',(4.49999999999401,69.6242977306766,-62.9424583655132));
#31223=CARTESIAN_POINT('Ctrl Pts',(10.6602540378348,68.8640022192353,-58.2600000000009));
#31224=CARTESIAN_POINT('Ctrl Pts',(10.248704850567,68.8065096163321,-58.9728241021613));
#31225=CARTESIAN_POINT('Ctrl Pts',(9.75221352104281,68.7599390932012,-59.6251196466602));
#31226=CARTESIAN_POINT('Ctrl Pts',(8.83757091267963,68.7439037327988,-60.5769028187122));
#31227=CARTESIAN_POINT('Ctrl Pts',(8.39639094390703,68.7544489459965,-60.9689841103285));
#31228=CARTESIAN_POINT('Ctrl Pts',(7.45384509647339,68.8392168199242,-61.6622512795055));
#31229=CARTESIAN_POINT('Ctrl Pts',(6.95262696745016,68.9146735330389,-61.9634865839287));
#31230=CARTESIAN_POINT('Ctrl Pts',(5.86111154267866,69.1490964557957,-62.5104810158789));
#31231=CARTESIAN_POINT('Ctrl Pts',(5.18034932187989,69.3490828791313,-62.766792925962));
#31232=CARTESIAN_POINT('Ctrl Pts',(4.49999999999421,69.6242977306766,-62.9424583655131));
#31233=CARTESIAN_POINT('Ctrl Pts',(4.49999999999909,69.6242977306746,-62.9424583655118));
#31234=CARTESIAN_POINT('Ctrl Pts',(3.6938450265894,69.950403473993,-63.1506066846109));
#31235=CARTESIAN_POINT('Ctrl Pts',(2.8431330228302,70.1896440739217,-63.2599999999947));
#31236=CARTESIAN_POINT('Ctrl Pts',(1.37467804558015,70.4378582683016,-63.2599999999947));
#31237=CARTESIAN_POINT('Ctrl Pts',(0.727224534423085,70.4951788900757,-63.2002681824217));
#31238=CARTESIAN_POINT('Ctrl Pts',(-0.558312959174255,70.5042267042902,
-62.9493716889925));
#31239=CARTESIAN_POINT('Ctrl Pts',(-1.19640226162106,70.4560846742305,-62.7582390058393));
#31240=CARTESIAN_POINT('Ctrl Pts',(-2.80448010483271,70.2113780440741,-62.0965365584756));
#31241=CARTESIAN_POINT('Ctrl Pts',(-3.72705357784681,69.9369699535809,-61.5204719079205));
#31242=CARTESIAN_POINT('Ctrl Pts',(-4.4999999999832,69.6242977306852,-60.8593420767994));
#31243=CARTESIAN_POINT('',(-6.66025403785039,70.5000000000327,-58.2599999999947));
#31244=CARTESIAN_POINT('Origin',(8.99999999999307,80.7485954613122,-137.259999999996));
#31245=CARTESIAN_POINT('',(13.499999999994,69.6242977306784,-53.3414157129525));
#31246=CARTESIAN_POINT('Origin',(9.00000000008001,80.748595461022,-61.1356443468633));
#31247=CARTESIAN_POINT('',(13.499999999994,69.6242977306697,-131.178584287037));
#31248=CARTESIAN_POINT('',(13.4999999999941,69.624297730669,-137.259999999995));
#31249=CARTESIAN_POINT('',(10.6602540378385,68.8640022192282,-126.259999999995));
#31250=CARTESIAN_POINT('Origin',(8.99999999987123,80.7485954618345,-123.384355652776));
#31251=CARTESIAN_POINT('',(4.49999999999396,69.62429773067,-121.577541634476));
#31252=CARTESIAN_POINT('Ctrl Pts',(10.6602540378386,68.8640022192282,-126.259999999995));
#31253=CARTESIAN_POINT('Ctrl Pts',(10.6511405690506,68.8627290857649,-126.24421500902));
#31254=CARTESIAN_POINT('Ctrl Pts',(10.6420002974861,68.8614628960272,-126.228483263499));
#31255=CARTESIAN_POINT('Ctrl Pts',(10.219407479571,68.8034210642394,-125.505671077853));
#31256=CARTESIAN_POINT('Ctrl Pts',(9.67726187597146,68.7512246263665,-124.79116967751));
#31257=CARTESIAN_POINT('Ctrl Pts',(8.4193522322561,68.7461607613385,-123.54131924113));
#31258=CARTESIAN_POINT('Ctrl Pts',(7.70358433234451,68.7975084367052,-123.00596056583));
#31259=CARTESIAN_POINT('Ctrl Pts',(6.26432228327072,69.040788125594,-122.175002234363));
#31260=CARTESIAN_POINT('Ctrl Pts',(5.42432246719667,69.2588498443473,-121.825186221089));
#31261=CARTESIAN_POINT('Ctrl Pts',(4.56168799981022,69.5994929078332,-121.593626545806));
#31262=CARTESIAN_POINT('Ctrl Pts',(4.53083553750895,69.6118241415791,-121.585503336027));
#31263=CARTESIAN_POINT('Ctrl Pts',(4.49999999998978,69.6242977306718,-121.577541634475));
#31264=CARTESIAN_POINT('',(4.49999999999401,69.6242977306683,-137.259999999995));
#31265=CARTESIAN_POINT('Origin',(1.11022302462516E-12,-11.1689999999848,
-213.999999999986));
#31266=CARTESIAN_POINT('',(-59.3192302506006,22.0759834182112,-211.880711975822));
#31267=CARTESIAN_POINT('',(-59.3192302505947,-44.4139834181905,-211.880711975815));
#31268=CARTESIAN_POINT('Origin',(1.11022302462516E-12,-11.1689999999845,
-211.880711975818));
#31269=CARTESIAN_POINT('',(-58.1696747238564,-60.8533933496133,-213.999999999979));
#31270=CARTESIAN_POINT('Ctrl Pts',(-59.3192302505947,-44.4139834181905,
-211.880711975815));
#31271=CARTESIAN_POINT('Ctrl Pts',(-58.7782629438943,-52.1501763270953,
-212.706060413095));
#31272=CARTESIAN_POINT('Ctrl Pts',(-58.1696747238564,-60.8533933496133,
-213.99999999998));
#31273=CARTESIAN_POINT('',(-49.6843933496171,-69.3386747238511,-213.999999999978));
#31274=CARTESIAN_POINT('Origin',(1.11022302462516E-12,-11.1689999999848,
-213.999999999986));
#31275=CARTESIAN_POINT('',(-33.2449834181943,-70.4882302505863,-211.880711975812));
#31276=CARTESIAN_POINT('Ctrl Pts',(-49.684393349617,-69.3386747238512,-213.999999999979));
#31277=CARTESIAN_POINT('Ctrl Pts',(-40.9811763270991,-69.9472629438874,
-212.706060413093));
#31278=CARTESIAN_POINT('Ctrl Pts',(-33.2449834181943,-70.4882302505863,
-211.880711975812));
#31279=CARTESIAN_POINT('',(33.2449834182069,-70.4882302505805,-211.880711975812));
#31280=CARTESIAN_POINT('Origin',(1.11022302462516E-12,-11.1689999999845,
-211.880711975818));
#31281=CARTESIAN_POINT('',(49.6843933496294,-69.3386747238425,-213.999999999978));
#31282=CARTESIAN_POINT('Ctrl Pts',(33.2449834182069,-70.4882302505805,-211.880711975812));
#31283=CARTESIAN_POINT('Ctrl Pts',(40.9811763271116,-69.9472629438803,-212.706060413093));
#31284=CARTESIAN_POINT('Ctrl Pts',(49.6843933496294,-69.3386747238425,-213.999999999979));
#31285=CARTESIAN_POINT('',(58.1696747238672,-60.8533933496032,-213.999999999979));
#31286=CARTESIAN_POINT('Origin',(1.11022302462516E-12,-11.1689999999848,
-213.999999999986));
#31287=CARTESIAN_POINT('',(59.3192302506027,-44.4139834181802,-211.880711975815));
#31288=CARTESIAN_POINT('Ctrl Pts',(58.1696747238672,-60.8533933496032,-213.99999999998));
#31289=CARTESIAN_POINT('Ctrl Pts',(58.7782629439037,-52.1501763270851,-212.706060413095));
#31290=CARTESIAN_POINT('Ctrl Pts',(59.3192302506027,-44.4139834181801,-211.880711975815));
#31291=CARTESIAN_POINT('',(68.0000000000011,-11.1689999999786,-211.880711975818));
#31292=CARTESIAN_POINT('Origin',(1.11022302462516E-12,-11.1689999999845,
-211.880711975818));
#31293=CARTESIAN_POINT('',(76.5000000000011,-11.1689999999781,-213.999999999986));
#31294=CARTESIAN_POINT('',(-52.4384165089406,-42.6312331099945,-210.173502450762));
#31295=CARTESIAN_POINT('Ctrl Pts',(-52.4384165089405,-42.6312331099945,
-210.173502450762));
#31296=CARTESIAN_POINT('Ctrl Pts',(-48.3519683114706,-40.9385708446668,
-209.082698564953));
#31297=CARTESIAN_POINT('Ctrl Pts',(-44.8103167727301,-39.4715707441205,
-208.140791933166));
#31298=CARTESIAN_POINT('',(-59.3267182915137,-26.0014015247919,-210.173502450764));
#31299=CARTESIAN_POINT('Ctrl Pts',(-52.4384165089406,-42.6312331099944,
-210.173502450762));
#31300=CARTESIAN_POINT('Ctrl Pts',(-55.9844712211047,-34.3585272620583,
-209.870455963678));
#31301=CARTESIAN_POINT('Ctrl Pts',(-59.3267182915136,-26.0014015247919,
-210.173502450764));
#31302=CARTESIAN_POINT('Ctrl Pts',(-59.3267182915137,-26.0014015247919,
-210.173502450764));
#31303=CARTESIAN_POINT('Ctrl Pts',(-55.2402700940438,-24.3087392594642,
-209.082698564955));
#31304=CARTESIAN_POINT('Ctrl Pts',(-51.6986185553031,-22.8417391589179,
-208.140791933168));
#31305=CARTESIAN_POINT('',(59.3192302505969,22.0759834182214,-211.880711975822));
#31306=CARTESIAN_POINT('Origin',(1.11022302462516E-12,-11.1689999999845,
-211.880711975818));
#31307=CARTESIAN_POINT('',(58.1696747238586,38.5153933496439,-213.999999999991));
#31308=CARTESIAN_POINT('Ctrl Pts',(59.3192302505969,22.0759834182215,-211.880711975822));
#31309=CARTESIAN_POINT('Ctrl Pts',(58.7782629438965,29.8121763271262,-212.706060413104));
#31310=CARTESIAN_POINT('Ctrl Pts',(58.1696747238585,38.5153933496438,-213.999999999991));
#31311=CARTESIAN_POINT('',(49.6843933496193,47.0006747238816,-213.999999999992));
#31312=CARTESIAN_POINT('Origin',(1.11022302462516E-12,-11.1689999999848,
-213.999999999986));
#31313=CARTESIAN_POINT('',(33.2449834181965,48.1502302506173,-211.880711975825));
#31314=CARTESIAN_POINT('Ctrl Pts',(49.6843933496193,47.0006747238816,-213.999999999992));
#31315=CARTESIAN_POINT('Ctrl Pts',(40.9811763271013,47.6092629439181,-212.706060413106));
#31316=CARTESIAN_POINT('Ctrl Pts',(33.2449834181965,48.1502302506173,-211.880711975825));
#31317=CARTESIAN_POINT('',(-33.2449834182046,48.1502302506115,-211.880711975825));
#31318=CARTESIAN_POINT('Origin',(1.11022302462516E-12,-11.1689999999845,
-211.880711975818));
#31319=CARTESIAN_POINT('',(-49.6843933496272,47.000674723873,-213.999999999992));
#31320=CARTESIAN_POINT('Ctrl Pts',(-33.2449834182046,48.1502302506115,-211.880711975825));
#31321=CARTESIAN_POINT('Ctrl Pts',(-40.9811763271093,47.609262943911,-212.706060413106));
#31322=CARTESIAN_POINT('Ctrl Pts',(-49.6843933496272,47.000674723873,-213.999999999992));
#31323=CARTESIAN_POINT('',(-58.169674723865,38.5153933496337,-213.999999999991));
#31324=CARTESIAN_POINT('Origin',(1.11022302462516E-12,-11.1689999999848,
-213.999999999986));
#31325=CARTESIAN_POINT('Ctrl Pts',(-58.169674723865,38.5153933496337,-213.999999999991));
#31326=CARTESIAN_POINT('Ctrl Pts',(-58.7782629439015,29.8121763271159,-212.706060413104));
#31327=CARTESIAN_POINT('Ctrl Pts',(-59.3192302506005,22.0759834182111,-211.880711975822));
#31328=CARTESIAN_POINT('',(-59.2516966812877,-34.5416704979166,-210.807339776632));
#31329=CARTESIAN_POINT('',(-58.341412086245,-36.6160882438761,-210.796041473035));
#31330=CARTESIAN_POINT('Ctrl Pts',(-59.2516966813201,-34.5416704957383,
-210.807339776229));
#31331=CARTESIAN_POINT('Ctrl Pts',(-59.029454981385,-34.5478031947605,-210.75635515438));
#31332=CARTESIAN_POINT('Ctrl Pts',(-58.7921795388409,-34.5649224930198,
-210.702930314816));
#31333=CARTESIAN_POINT('Ctrl Pts',(-58.4366785026112,-34.6298287310412,
-210.626651867582));
#31334=CARTESIAN_POINT('Ctrl Pts',(-58.312197261563,-34.6607888434274,-210.600732341974));
#31335=CARTESIAN_POINT('Ctrl Pts',(-58.0781686614658,-34.747530321667,-210.554747021162));
#31336=CARTESIAN_POINT('Ctrl Pts',(-57.9682517418723,-34.8022087259218,
-210.534489049959));
#31337=CARTESIAN_POINT('Ctrl Pts',(-57.8331509870804,-34.9164071144292,
-210.514115724432));
#31338=CARTESIAN_POINT('Ctrl Pts',(-57.7935864618605,-34.9574272928331,
-210.508879171898));
#31339=CARTESIAN_POINT('Ctrl Pts',(-57.7287600318386,-35.0494073869723,
-210.502685784877));
#31340=CARTESIAN_POINT('Ctrl Pts',(-57.7036583364591,-35.1004833661575,
-210.501777404252));
#31341=CARTESIAN_POINT('Ctrl Pts',(-57.6694577754129,-35.2056166064024,
-210.503965499983));
#31342=CARTESIAN_POINT('Ctrl Pts',(-57.6596154308036,-35.2682318542073,
-210.507714108404));
#31343=CARTESIAN_POINT('Ctrl Pts',(-57.6582870250246,-35.3939331364455,
-210.519521527325));
#31344=CARTESIAN_POINT('Ctrl Pts',(-57.6664633243023,-35.4570226989156,
-210.527502248886));
#31345=CARTESIAN_POINT('Ctrl Pts',(-57.7016594788991,-35.621513122669,-210.551534754846));
#31346=CARTESIAN_POINT('Ctrl Pts',(-57.7386665647023,-35.7159198006795,
-210.569232984154));
#31347=CARTESIAN_POINT('Ctrl Pts',(-57.8204746085682,-35.8913905023802,
-210.605154351717));
#31348=CARTESIAN_POINT('Ctrl Pts',(-57.8659994434101,-35.9720888655669,
-210.623510416932));
#31349=CARTESIAN_POINT('Ctrl Pts',(-58.0089417708346,-36.2023684566477,
-210.678918981039));
#31350=CARTESIAN_POINT('Ctrl Pts',(-58.1120369384791,-36.3394897776198,
-210.716089360605));
#31351=CARTESIAN_POINT('Ctrl Pts',(-58.2591150958127,-36.5199599816261,
-210.767655854534));
#31352=CARTESIAN_POINT('Ctrl Pts',(-58.3000784572093,-36.5684840123265,
-210.781850056857));
#31353=CARTESIAN_POINT('Ctrl Pts',(-58.3414120848803,-36.6160882451689,
-210.796041472673));
#31354=CARTESIAN_POINT('Ctrl Pts',(-58.3414120868986,-36.616088244313,-210.796041473049));
#31355=CARTESIAN_POINT('Ctrl Pts',(-58.5196070612518,-36.3488442716846,
-210.810126004893));
#31356=CARTESIAN_POINT('Ctrl Pts',(-58.6856862024724,-36.0599520454846,
-210.819863004671));
#31357=CARTESIAN_POINT('Ctrl Pts',(-59.0239120577606,-35.331588505113,-210.827688366328));
#31358=CARTESIAN_POINT('Ctrl Pts',(-59.1566032891731,-34.9319981002169,
-210.82099539984));
#31359=CARTESIAN_POINT('Ctrl Pts',(-59.2516966823843,-34.5416704981807,
-210.807339776699));
#31360=CARTESIAN_POINT('Origin',(-59.506244168816,-35.8520251485972,-203.77397811514));
#31361=CARTESIAN_POINT('',(-54.7302932280859,-40.0172481069749,-207.104324991779));
#31362=CARTESIAN_POINT('',(-61.6687352492389,-30.9288598303485,-199.047872363436));
#31363=CARTESIAN_POINT('Origin',(-58.1950257608775,-35.2740441834793,-203.296733644058));
#31364=CARTESIAN_POINT('',(-61.0274459660746,-28.8726777694807,-203.299999999994));
#31365=CARTESIAN_POINT('Origin',(-58.2040000000275,-35.2780000000021,-203.299999999994));
#31366=CARTESIAN_POINT('',(-63.6319343036514,-30.0207280666708,-204.247956230286));
#31367=CARTESIAN_POINT('',(-62.3296901348632,-29.4467029180758,-203.77397811514));
#31368=CARTESIAN_POINT('Origin',(-60.8084883376043,-36.4260502971922,-204.247956230285));
#31369=CARTESIAN_POINT('Origin',(-60.8084883376043,-36.4260502971922,-204.247956230285));
#31370=CARTESIAN_POINT('Origin',(-58.2040000000275,-35.2780000000021,-203.299999999994));
#31371=CARTESIAN_POINT('Origin',(26.9999999999931,80.7485954613137,-137.259999999996));
#31372=CARTESIAN_POINT('',(31.499999999994,69.6242977306766,-84.2599999999946));
#31373=CARTESIAN_POINT('',(22.4999999999941,69.6242977306758,-84.2599999999946));
#31374=CARTESIAN_POINT('Origin',(26.9999999999931,80.7485954613196,-84.2599999999958));
#31375=CARTESIAN_POINT('',(31.499999999994,69.6242977306748,-100.259999999995));
#31376=CARTESIAN_POINT('',(31.499999999994,69.6242977306707,-137.259999999995));
#31377=CARTESIAN_POINT('',(22.4999999999941,69.624297730674,-100.259999999995));
#31378=CARTESIAN_POINT('Origin',(26.9999999999931,80.7485954613179,-100.259999999996));
#31379=CARTESIAN_POINT('',(22.4999999999941,69.6242977306698,-137.259999999995));
#31380=CARTESIAN_POINT('Origin',(1.11022302462516E-12,-11.1689999999872,
-235.499999999986));
#31381=CARTESIAN_POINT('',(32.4575348647363,48.5847315195132,-232.499999999992));
#31382=CARTESIAN_POINT('',(-32.4575348647446,48.5847315195076,-232.499999999992));
#31383=CARTESIAN_POINT('Origin',(1.11022302462516E-12,-11.1689999999869,
-232.499999999986));
#31384=CARTESIAN_POINT('',(-32.4575348647445,48.5847315195081,-227.499999999992));
#31385=CARTESIAN_POINT('',(-32.4575348647446,48.5847315195072,-235.499999999992));
#31386=CARTESIAN_POINT('',(-33.2449834182046,48.1502302506097,-227.499999999992));
#31387=CARTESIAN_POINT('Origin',(1.11022302462516E-12,-11.1689999999863,
-227.499999999986));
#31388=CARTESIAN_POINT('',(-33.2449834182046,48.150230250612,-207.499999999949));
#31389=CARTESIAN_POINT('',(33.2449834181965,48.1502302506155,-227.499999999992));
#31390=CARTESIAN_POINT('',(33.2449834181965,48.1502302506146,-235.499999999992));
#31391=CARTESIAN_POINT('',(32.4575348647363,48.5847315195138,-227.499999999992));
#31392=CARTESIAN_POINT('Origin',(1.11022302462516E-12,-11.1689999999863,
-227.499999999986));
#31393=CARTESIAN_POINT('',(32.4575348647363,48.5847315195129,-235.499999999992));
#31394=CARTESIAN_POINT('Origin',(-60.8084883376896,-36.4260502972298,-204.247956230316));
#31395=CARTESIAN_POINT('',(-64.0967476590949,-31.3184575319747,-204.563941640371));
#31396=CARTESIAN_POINT('',(-63.6319343036976,-30.0207280667973,-204.247956230317));
#31397=CARTESIAN_POINT('Origin',(-61.6766511167642,-36.8087337295747,-204.56394164037));
#31398=CARTESIAN_POINT('Origin',(6.77236045021346E-12,-76.1689999999813,
-183.999999999978));
#31399=CARTESIAN_POINT('',(7.12190442787529E-12,-80.1689999999816,-186.499999999978));
#31400=CARTESIAN_POINT('Origin',(6.77236045021346E-12,-76.1689999999816,
-186.499999999978));
#31401=CARTESIAN_POINT('',(7.12190442787524E-12,-80.168999999981,-181.499999999978));
#31402=CARTESIAN_POINT('',(7.12190442787527E-12,-80.1689999999813,-183.999999999978));
#31403=CARTESIAN_POINT('Origin',(6.77236045021346E-12,-76.168999999981,
-181.499999999978));
#31404=CARTESIAN_POINT('Origin',(65.0000000000011,-11.1689999999756,-183.999999999986));
#31405=CARTESIAN_POINT('',(65.0000000000014,-15.1689999999759,-186.499999999985));
#31406=CARTESIAN_POINT('Origin',(65.0000000000011,-11.1689999999759,-186.499999999986));
#31407=CARTESIAN_POINT('',(65.0000000000014,-15.1689999999753,-181.499999999985));
#31408=CARTESIAN_POINT('',(65.0000000000014,-15.1689999999756,-183.999999999985));
#31409=CARTESIAN_POINT('Origin',(65.0000000000011,-11.1689999999753,-181.499999999986));
#31410=CARTESIAN_POINT('Origin',(-4.57966997657877E-12,53.8310000000187,
-183.999999999993));
#31411=CARTESIAN_POINT('',(-4.23012599891694E-12,49.8310000000184,-186.499999999993));
#31412=CARTESIAN_POINT('Origin',(-4.57966997657877E-12,53.8310000000184,
-186.499999999993));
#31413=CARTESIAN_POINT('',(-4.23012599891699E-12,49.831000000019,-181.499999999993));
#31414=CARTESIAN_POINT('',(-4.23012599891696E-12,49.8310000000187,-183.999999999993));
#31415=CARTESIAN_POINT('Origin',(-4.57966997657877E-12,53.831000000019,
-181.499999999993));
#31416=CARTESIAN_POINT('Origin',(-64.9999999999989,-11.1689999999869,-183.999999999986));
#31417=CARTESIAN_POINT('',(-64.9999999999986,-15.1689999999872,-186.499999999985));
#31418=CARTESIAN_POINT('Origin',(-64.9999999999989,-11.1689999999873,-186.499999999986));
#31419=CARTESIAN_POINT('',(-64.9999999999986,-15.1689999999867,-181.499999999985));
#31420=CARTESIAN_POINT('',(-64.9999999999986,-15.1689999999869,-183.999999999985));
#31421=CARTESIAN_POINT('Origin',(-64.9999999999989,-11.1689999999867,-181.499999999986));
#31422=CARTESIAN_POINT('Origin',(1.11022302462516E-13,4.3869638824412E-11,
34.5000000000134));
#31423=CARTESIAN_POINT('',(-1.41067854607095E-12,17.4625000000399,1.13953291247526E-11));
#31424=CARTESIAN_POINT('Origin',(1.11022302462516E-13,3.99005915113771E-11,
1.34059430223488E-11));
#31425=CARTESIAN_POINT('',(-1.41067854607102E-12,17.4625000000407,7.0000000000114));
#31426=CARTESIAN_POINT('',(-1.41067854607129E-12,17.4625000000439,34.5000000000114));
#31427=CARTESIAN_POINT('',(3.96999999999864,17.0052346720472,7.00000000001144));
#31428=CARTESIAN_POINT('Origin',(1.11022302462516E-13,4.07055032042302E-11,
7.00000000001341));
#31429=CARTESIAN_POINT('',(3.96999999999864,17.0052346720536,63.0000000000114));
#31430=CARTESIAN_POINT('',(3.96999999999864,17.0052346720503,34.5000000000115));
#31431=CARTESIAN_POINT('',(-1.41067854607158E-12,17.4625000000471,63.0000000000114));
#31432=CARTESIAN_POINT('Origin',(1.11022302462516E-13,4.71447967470562E-11,
63.0000000000134));
#31433=CARTESIAN_POINT('',(-1.41067854607164E-12,17.4625000000478,69.0000000000114));
#31434=CARTESIAN_POINT('',(-1.41067854607129E-12,17.4625000000439,34.5000000000114));
#31435=CARTESIAN_POINT('Origin',(1.11022302462516E-13,4.78386861374469E-11,
69.0000000000134));
#31436=CARTESIAN_POINT('',(-3.97000000000136,17.005234672053,63.0000000000114));
#31437=CARTESIAN_POINT('Origin',(1.11022302462516E-13,4.71447967470562E-11,
63.0000000000134));
#31438=CARTESIAN_POINT('',(-3.97000000000136,17.0052346720466,7.00000000001144));
#31439=CARTESIAN_POINT('',(-3.97000000000136,17.0052346720497,34.5000000000115));
#31440=CARTESIAN_POINT('Origin',(1.11022302462516E-13,4.07055032042302E-11,
7.00000000001341));
#31441=CARTESIAN_POINT('Origin',(26.999999999994,70.5000000000298,-110.759999999995));
#31442=CARTESIAN_POINT('',(26.9999999999943,67.0000000000306,-102.759999999994));
#31443=CARTESIAN_POINT('Origin',(26.9999999999943,67.0000000000297,-110.759999999994));
#31444=CARTESIAN_POINT('',(26.999999999994,70.5000000000306,-102.759999999995));
#31445=CARTESIAN_POINT('',(26.999999999994,70.5000000000307,-102.759999999995));
#31446=CARTESIAN_POINT('Origin',(26.999999999994,70.5000000000297,-110.759999999995));
#31447=CARTESIAN_POINT('Origin',(26.9899999999939,70.5000000000338,-73.7599999999947));
#31448=CARTESIAN_POINT('',(26.9899999999943,67.0000000000347,-65.7599999999943));
#31449=CARTESIAN_POINT('Origin',(26.9899999999942,67.0000000000338,-73.7599999999943));
#31450=CARTESIAN_POINT('',(26.9899999999939,70.5000000000348,-65.7599999999947));
#31451=CARTESIAN_POINT('',(26.9899999999939,70.5000000000347,-65.7599999999947));
#31452=CARTESIAN_POINT('Origin',(26.9899999999939,70.5000000000339,-73.7599999999947));
#31453=CARTESIAN_POINT('Origin',(1.11022302462516E-13,4.78386861374469E-11,
69.0000000000134));
#31454=CARTESIAN_POINT('',(-1.32353748101568E-12,16.4625000000479,70.0000000000115));
#31455=CARTESIAN_POINT('',(-1.41067854607129E-12,17.4625000000478,69.0000000000114));
#31456=CARTESIAN_POINT('Origin',(1.11022302462516E-13,4.79774640155251E-11,
70.0000000000134));
#31457=CARTESIAN_POINT('Origin',(26.9999999999943,67.0000000000295,-110.759999999994));
#31458=CARTESIAN_POINT('',(26.9999999999943,67.0000000000289,-117.759999999994));
#31459=CARTESIAN_POINT('Origin',(26.9999999999943,67.0000000000297,-110.759999999994));
#31460=CARTESIAN_POINT('',(26.9999999999939,71.0000000000287,-117.759999999995));
#31461=CARTESIAN_POINT('',(26.9999999999943,67.0000000000287,-117.759999999994));
#31462=CARTESIAN_POINT('Origin',(26.9999999999939,71.0000000000295,-110.759999999995));
#31463=CARTESIAN_POINT('Origin',(26.9899999999942,67.0000000000338,-73.7599999999943));
#31464=CARTESIAN_POINT('',(26.9899999999942,67.000000000033,-80.7599999999943));
#31465=CARTESIAN_POINT('Origin',(26.9899999999942,67.0000000000338,-73.7599999999943));
#31466=CARTESIAN_POINT('',(26.9899999999939,71.000000000033,-80.7599999999948));
#31467=CARTESIAN_POINT('',(26.9899999999942,67.000000000033,-80.7599999999943));
#31468=CARTESIAN_POINT('Origin',(26.9899999999939,71.0000000000338,-73.7599999999948));
#31469=CARTESIAN_POINT('Origin',(-50.5581348548326,-61.7271348548489,-400.985281374227));
#31470=CARTESIAN_POINT('',(-50.5581348548323,-64.7271348548299,-235.499999999979));
#31471=CARTESIAN_POINT('Origin',(-50.5581348548326,-61.7271348548299,-235.49999999998));
#31472=CARTESIAN_POINT('',(-50.5581348548323,-64.7271348548479,-392.499999999979));
#31473=CARTESIAN_POINT('',(-50.5581348548323,-64.7271348548489,-400.985281374226));
#31474=CARTESIAN_POINT('Origin',(-50.5581348548326,-61.7271348548479,-392.49999999998));
#31475=CARTESIAN_POINT('Origin',(-50.5581348548387,39.3891348548274,-400.985281374238));
#31476=CARTESIAN_POINT('',(-50.5581348548384,36.3891348548434,-235.499999999991));
#31477=CARTESIAN_POINT('Origin',(-50.5581348548387,39.3891348548464,-235.499999999991));
#31478=CARTESIAN_POINT('',(-50.5581348548384,36.3891348548253,-392.499999999991));
#31479=CARTESIAN_POINT('',(-50.5581348548384,36.3891348548243,-400.985281374238));
#31480=CARTESIAN_POINT('Origin',(-50.5581348548387,39.3891348548284,-392.499999999991));
#31481=CARTESIAN_POINT('Origin',(50.5581348548376,39.3891348548335,-400.985281374238));
#31482=CARTESIAN_POINT('',(50.5581348548379,36.3891348548505,-235.499999999991));
#31483=CARTESIAN_POINT('Origin',(50.5581348548376,39.3891348548526,-235.499999999991));
#31484=CARTESIAN_POINT('',(50.5581348548379,36.3891348548324,-392.499999999991));
#31485=CARTESIAN_POINT('',(50.5581348548379,36.3891348548314,-400.985281374238));
#31486=CARTESIAN_POINT('Origin',(50.5581348548376,39.3891348548345,-392.499999999991));
#31487=CARTESIAN_POINT('Origin',(50.5581348548437,-61.7271348548428,-400.985281374227));
#31488=CARTESIAN_POINT('',(50.558134854844,-64.727134854823,-235.499999999979));
#31489=CARTESIAN_POINT('Origin',(50.5581348548437,-61.7271348548237,-235.49999999998));
#31490=CARTESIAN_POINT('',(50.558134854844,-64.7271348548411,-392.499999999979));
#31491=CARTESIAN_POINT('',(50.558134854844,-64.7271348548421,-400.985281374226));
#31492=CARTESIAN_POINT('Origin',(50.5581348548437,-61.7271348548418,-392.49999999998));
#31493=CARTESIAN_POINT('Origin',(1.11022302462516E-12,-11.1690000000053,
-392.499999999986));
#31494=CARTESIAN_POINT('',(32.4575348647468,-70.9227315195001,-395.499999999979));
#31495=CARTESIAN_POINT('',(-32.4575348647341,-70.9227315195058,-395.499999999979));
#31496=CARTESIAN_POINT('Origin',(1.11022302462516E-12,-11.1690000000057,
-395.499999999985));
#31497=CARTESIAN_POINT('',(-32.4575348647341,-70.9227315195064,-400.499999999979));
#31498=CARTESIAN_POINT('',(-32.4575348647342,-70.9227315195055,-392.499999999978));
#31499=CARTESIAN_POINT('',(32.4575348647468,-70.9227315195007,-400.499999999979));
#31500=CARTESIAN_POINT('Origin',(1.11022302462516E-12,-11.1690000000062,
-400.499999999986));
#31501=CARTESIAN_POINT('',(32.4575348647468,-70.9227315194997,-392.499999999978));
#31502=CARTESIAN_POINT('Origin',(1.11022302462516E-13,4.71170411714406E-11,
62.6499999999764));
#31503=CARTESIAN_POINT('',(-4.77179886666E-13,6.75000000008227,60.5000000000126));
#31504=CARTESIAN_POINT('',(-4.77179886666022E-13,6.75000000008252,62.6499999999756));
#31505=CARTESIAN_POINT('',(-6.75000000002784,4.62773855285951E-11,60.5000000000209));
#31506=CARTESIAN_POINT('Origin',(1.11022302462516E-13,4.68672409908999E-11,
60.5000000000134));
#31507=CARTESIAN_POINT('Origin',(1.11022302462516E-13,4.68672409908999E-11,
60.5000000000134));
#31508=CARTESIAN_POINT('Origin',(-871.,-11.1690000000814,-400.499999999982));
#31509=CARTESIAN_POINT('',(72.525443681756,-54.5019036555836,-427.999999999988));
#31510=CARTESIAN_POINT('',(72.5254436817485,32.1639036555757,-428.));
#31511=CARTESIAN_POINT('Origin',(-871.,-11.1690000000845,-427.99999999999));
#31512=CARTESIAN_POINT('',(73.0049525312962,32.1859258606169,-400.499999999992));
#31513=CARTESIAN_POINT('',(73.0049525312962,32.1859258606169,-400.499999999992));
#31514=CARTESIAN_POINT('',(73.004952531304,-54.5239258606185,-400.499999999982));
#31515=CARTESIAN_POINT('Origin',(-871.,-11.1690000000814,-400.499999999979));
#31516=CARTESIAN_POINT('',(73.004952531304,-54.5239258606185,-400.499999999984));
#31517=CARTESIAN_POINT('Origin',(1.11022302462516E-13,4.68672409908999E-11,
60.5000000000038));
#31518=CARTESIAN_POINT('',(5.91645271747417E-13,-5.49999999995327,59.2499999999771));
#31519=CARTESIAN_POINT('',(-5.4999999999835,4.62426359731071E-11,59.2499999999765));
#31520=CARTESIAN_POINT('Origin',(1.11022302462516E-13,4.67284631128218E-11,
59.2499999999765));
#31521=CARTESIAN_POINT('Origin',(1.11022302462516E-13,4.67284631128218E-11,
59.2499999999765));
#31522=CARTESIAN_POINT('',(-6.7500000000108,4.62773855285947E-11,60.5000000000038));
#31523=CARTESIAN_POINT('Origin',(1.11022302462516E-13,4.57570179662747E-11,
50.8000000000134));
#31524=CARTESIAN_POINT('',(-4.06739714446706E-13,5.50000000004478,42.3500000000128));
#31525=CARTESIAN_POINT('',(5.91645271747587E-13,-5.49999999995522,42.350000000014));
#31526=CARTESIAN_POINT('Origin',(1.11022302462516E-13,4.47855728197277E-11,
42.3500000000134));
#31527=CARTESIAN_POINT('Origin',(1.11022302462516E-13,4.47855728197277E-11,
42.3500000000134));
#31528=CARTESIAN_POINT('',(5.91645271747502E-13,-5.49999999995424,50.800000000014));
#31529=CARTESIAN_POINT('Origin',(-871.,-11.1690000000846,-427.999999999983));
#31530=CARTESIAN_POINT('',(70.7822037839096,-15.3837757183187,-439.937224614355));
#31531=CARTESIAN_POINT('',(70.7822037837444,-6.95422428207094,-439.937224614869));
#31532=CARTESIAN_POINT('Ctrl Pts',(70.7822037837443,-15.3837757179392,-439.937224614868));
#31533=CARTESIAN_POINT('Ctrl Pts',(70.7793815670799,-14.7181872564058,-440.26955676224));
#31534=CARTESIAN_POINT('Ctrl Pts',(70.7771136682848,-14.0238576141718,-440.537081066418));
#31535=CARTESIAN_POINT('Ctrl Pts',(70.7740765236161,-12.6025387021907,-440.895543254428));
#31536=CARTESIAN_POINT('Ctrl Pts',(70.773294912811,-11.8913254701458,-440.987905442524));
#31537=CARTESIAN_POINT('Ctrl Pts',(70.7732942454401,-10.4474454821257,-440.987984275525));
#31538=CARTESIAN_POINT('Ctrl Pts',(70.7740755308484,-9.73607650775737,-440.8956604892));
#31539=CARTESIAN_POINT('Ctrl Pts',(70.7771127074938,-8.31443689341987,-440.537194400521));
#31540=CARTESIAN_POINT('Ctrl Pts',(70.7793809661231,-7.61995447243546,-440.269627528263));
#31541=CARTESIAN_POINT('Ctrl Pts',(70.7822037837436,-6.9542242820708,-439.93722461487));
#31542=CARTESIAN_POINT('',(70.7804124467087,-3.96116868056053,-438.999999999988));
#31543=CARTESIAN_POINT('Ctrl Pts',(70.7822037837436,-6.95422428207028,-439.93722461487));
#31544=CARTESIAN_POINT('Ctrl Pts',(70.784260001646,-6.47662207653906,-439.696973540908));
#31545=CARTESIAN_POINT('Ctrl Pts',(70.7852286730449,-5.98180724382513,-439.493770109462));
#31546=CARTESIAN_POINT('Ctrl Pts',(70.7846425695099,-4.97817312280563,-439.179518622343));
#31547=CARTESIAN_POINT('Ctrl Pts',(70.7831704772474,-4.47390580694272,-439.066807118521));
#31548=CARTESIAN_POINT('Ctrl Pts',(70.7804124467078,-3.96116868056048,-438.999999999988));
#31549=CARTESIAN_POINT('',(70.761115158048,-1.77218793995686,-438.999999999987));
#31550=CARTESIAN_POINT('Origin',(-871.000107047341,-11.169000944124,-438.999998579555));
#31551=CARTESIAN_POINT('',(70.7115584312605,1.14064771598034,-439.915842225177));
#31552=CARTESIAN_POINT('Ctrl Pts',(70.7611151580471,-1.772187939957,-438.999999999989));
#31553=CARTESIAN_POINT('Ctrl Pts',(70.7549712858817,-1.2712400283809,-439.065619900641));
#31554=CARTESIAN_POINT('Ctrl Pts',(70.7477342419649,-0.778729462480956,
-439.175730874464));
#31555=CARTESIAN_POINT('Ctrl Pts',(70.7310929468594,0.198249032937304,-439.482912240457));
#31556=CARTESIAN_POINT('Ctrl Pts',(70.7217076382667,0.677934742452566,-439.68092633614));
#31557=CARTESIAN_POINT('Ctrl Pts',(70.7115584312596,1.14064771597983,-439.915842225178));
#31558=CARTESIAN_POINT('',(70.5621815020405,9.72878593023437,-439.798062313339));
#31559=CARTESIAN_POINT('Ctrl Pts',(70.7115584312596,1.14064771598,-439.915842225178));
#31560=CARTESIAN_POINT('Ctrl Pts',(70.6977555438623,1.7722760085199,-440.233574685584));
#31561=CARTESIAN_POINT('Ctrl Pts',(70.6841784180189,2.43135220063798,-440.481498690251));
#31562=CARTESIAN_POINT('Ctrl Pts',(70.6576559190849,3.79836391559058,-440.812682544676));
#31563=CARTESIAN_POINT('Ctrl Pts',(70.6450375971601,4.48847501002298,-440.893489401533));
#31564=CARTESIAN_POINT('Ctrl Pts',(70.6195899340406,5.95683448888694,-440.890104980619));
#31565=CARTESIAN_POINT('Ctrl Pts',(70.6072142402067,6.7166479370343,-440.788838196047));
#31566=CARTESIAN_POINT('Ctrl Pts',(70.5835347472419,8.24335729001911,-440.414736630433));
#31567=CARTESIAN_POINT('Ctrl Pts',(70.5724334125237,9.00060738974511,-440.13655505323));
#31568=CARTESIAN_POINT('Ctrl Pts',(70.5621815020397,9.72878593023391,-439.798062313338));
#31569=CARTESIAN_POINT('',(70.5123942581075,12.4256934496977,-438.999999999989));
#31570=CARTESIAN_POINT('Ctrl Pts',(70.5621815020397,9.72878593023386,-439.798062313338));
#31571=CARTESIAN_POINT('Ctrl Pts',(70.5560935286397,10.1630589717267,-439.594696903278));
#31572=CARTESIAN_POINT('Ctrl Pts',(70.5488623731821,10.6109112971744,-439.422304715381));
#31573=CARTESIAN_POINT('Ctrl Pts',(70.532189399423,11.5143833304763,-439.154979614465));
#31574=CARTESIAN_POINT('Ctrl Pts',(70.5228784997486,11.9667160576192,-439.058298484005));
#31575=CARTESIAN_POINT('Ctrl Pts',(70.5123942581067,12.4256934496978,-438.99999999999));
#31576=CARTESIAN_POINT('',(70.4593636589108,14.4545180952481,-438.999999999989));
#31577=CARTESIAN_POINT('Origin',(-871.000092098264,-11.1690024073961,-438.999997857804));
#31578=CARTESIAN_POINT('',(70.2929704410881,18.8989817281299,-441.000070380918));
#31579=CARTESIAN_POINT('Ctrl Pts',(70.4593636589101,14.454518095248,-438.99999999999));
#31580=CARTESIAN_POINT('Ctrl Pts',(70.4323968085906,15.3696263962396,-439.118003644213));
#31581=CARTESIAN_POINT('Ctrl Pts',(70.402361472674,16.2465973045633,-439.394182358811));
#31582=CARTESIAN_POINT('Ctrl Pts',(70.3451108148425,17.725685099839,-440.131591270883));
#31583=CARTESIAN_POINT('Ctrl Pts',(70.3190794500871,18.3352673501182,-440.536136589015));
#31584=CARTESIAN_POINT('Ctrl Pts',(70.292970440885,18.8989817282384,-441.000070380775));
#31585=CARTESIAN_POINT('',(69.7816652336224,32.0328182762798,-441.000100325617));
#31586=CARTESIAN_POINT('Ctrl Pts',(70.2929704408694,18.8989817281253,-441.000070381875));
#31587=CARTESIAN_POINT('Ctrl Pts',(70.2251073370001,21.0262639243397,-440.994959300743));
#31588=CARTESIAN_POINT('Ctrl Pts',(70.150003220528,23.1528067113153,-440.992592473935));
#31589=CARTESIAN_POINT('Ctrl Pts',(69.9804315445582,27.5309940661356,-440.992609031095));
#31590=CARTESIAN_POINT('Ctrl Pts',(69.8851070136805,29.7820605867228,-440.995276017104));
#31591=CARTESIAN_POINT('Ctrl Pts',(69.7816652336217,32.0328182762798,-441.000100325618));
#31592=CARTESIAN_POINT('',(70.0083439496798,32.0432276337977,-427.999999999994));
#31593=CARTESIAN_POINT('',(70.008342200333,32.0432275534655,-428.000100325617));
#31594=CARTESIAN_POINT('',(70.0083439496875,-54.3812276338044,-427.999999999984));
#31595=CARTESIAN_POINT('Origin',(-871.,-11.1690000000846,-427.999999999982));
#31596=CARTESIAN_POINT('',(69.7816652336299,-54.3708182762896,-441.000100325607));
#31597=CARTESIAN_POINT('',(70.0083439496874,-54.3812276338046,-427.999999999984));
#31598=CARTESIAN_POINT('',(70.2929704406237,-41.2369817304577,-441.000070382643));
#31599=CARTESIAN_POINT('Ctrl Pts',(69.7816652336292,-54.3708182762895,-441.000100325608));
#31600=CARTESIAN_POINT('Ctrl Pts',(69.8851070061175,-52.1200607514469,-440.995276017448));
#31601=CARTESIAN_POINT('Ctrl Pts',(69.9804315306073,-49.8689943957394,-440.992609031477));
#31602=CARTESIAN_POINT('Ctrl Pts',(70.1500033362218,-45.49080375343,-440.992592473549));
#31603=CARTESIAN_POINT('Ctrl Pts',(70.2251072266989,-43.3642673819341,-440.99495929243));
#31604=CARTESIAN_POINT('Ctrl Pts',(70.2929704408003,-41.2369817304615,-441.000070381863));
#31605=CARTESIAN_POINT('',(70.4593636589152,-36.7925180952641,-438.999999999984));
#31606=CARTESIAN_POINT('Ctrl Pts',(70.2929704407877,-41.2369817303642,-441.000070382765));
#31607=CARTESIAN_POINT('Ctrl Pts',(70.317704961237,-40.7029436632141,-440.560560029249));
#31608=CARTESIAN_POINT('Ctrl Pts',(70.3423766984901,-40.1275883461274,-440.17422668545));
#31609=CARTESIAN_POINT('Ctrl Pts',(70.399844103119,-38.6577652909441,-439.417647186168));
#31610=CARTESIAN_POINT('Ctrl Pts',(70.4312604023686,-37.7461955970541,-439.122967454739));
#31611=CARTESIAN_POINT('Ctrl Pts',(70.4593636589143,-36.7925180952639,-438.999999999984));
#31612=CARTESIAN_POINT('',(70.5123942581118,-34.7636934497019,-438.999999999984));
#31613=CARTESIAN_POINT('Origin',(-871.000092221015,-11.1689975899443,-438.99999810262));
#31614=CARTESIAN_POINT('',(70.5621815020439,-32.0667859302444,-439.798062313334));
#31615=CARTESIAN_POINT('Ctrl Pts',(70.5123942581109,-34.763693449702,-438.999999999984));
#31616=CARTESIAN_POINT('Ctrl Pts',(70.5244264243219,-34.2369512725135,-439.066905845301));
#31617=CARTESIAN_POINT('Ctrl Pts',(70.5349061547253,-33.7192548928422,-439.184327052031));
#31618=CARTESIAN_POINT('Ctrl Pts',(70.5508948328608,-32.8218972350616,-439.471919820818));
#31619=CARTESIAN_POINT('Ctrl Pts',(70.5569594113589,-32.4392930119041,-439.623621240154));
#31620=CARTESIAN_POINT('Ctrl Pts',(70.5621815020433,-32.0667859302438,-439.798062313332));
#31621=CARTESIAN_POINT('',(70.7115584312623,-23.4786477159905,-439.915842225175));
#31622=CARTESIAN_POINT('Ctrl Pts',(70.5621815020433,-32.066785930244,-439.798062313333));
#31623=CARTESIAN_POINT('Ctrl Pts',(70.579829006079,-30.8133089561511,-440.380739269272));
#31624=CARTESIAN_POINT('Ctrl Pts',(70.599849431034,-29.4823568207801,-440.780673806023));
#31625=CARTESIAN_POINT('Ctrl Pts',(70.6364529932775,-27.3071756279525,-440.924738336709));
#31626=CARTESIAN_POINT('Ctrl Pts',(70.6505405351955,-26.5176964957163,-440.873145899115));
#31627=CARTESIAN_POINT('Ctrl Pts',(70.6804876960852,-24.9493418204798,-440.547513202668));
#31628=CARTESIAN_POINT('Ctrl Pts',(70.6958611485221,-24.1969646600544,-440.277182292876));
#31629=CARTESIAN_POINT('Ctrl Pts',(70.7115584312618,-23.4786477159904,-439.915842225175));
#31630=CARTESIAN_POINT('',(70.7611151580495,-20.5658120600565,-438.999999999986));
#31631=CARTESIAN_POINT('Ctrl Pts',(70.7115584312618,-23.4786477159902,-439.915842225175));
#31632=CARTESIAN_POINT('Ctrl Pts',(70.7217087916647,-23.0158821579329,-439.680899639368));
#31633=CARTESIAN_POINT('Ctrl Pts',(70.7310950754517,-22.5361402088534,-439.482867337723));
#31634=CARTESIAN_POINT('Ctrl Pts',(70.7477359295614,-21.5591557455211,-439.175705187447));
#31635=CARTESIAN_POINT('Ctrl Pts',(70.7549720035577,-21.0667014551982,-439.065612235486));
#31636=CARTESIAN_POINT('Ctrl Pts',(70.7611151580486,-20.5658120600564,-438.999999999987));
#31637=CARTESIAN_POINT('',(70.7804124467098,-18.3768313194477,-438.999999999986));
#31638=CARTESIAN_POINT('Origin',(-871.000106910411,-11.1689990568951,-438.999998737379));
#31639=CARTESIAN_POINT('Ctrl Pts',(70.780412446709,-18.3768313194477,-438.999999999987));
#31640=CARTESIAN_POINT('Ctrl Pts',(70.7831704612649,-17.8640971645283,-439.066806731352));
#31641=CARTESIAN_POINT('Ctrl Pts',(70.7846425525253,-17.359832709541,-439.179517317669));
#31642=CARTESIAN_POINT('Ctrl Pts',(70.7852286838526,-16.3561982906056,-439.493767837466));
#31643=CARTESIAN_POINT('Ctrl Pts',(70.7842600131655,-15.8613805991198,-439.696972194992));
#31644=CARTESIAN_POINT('Ctrl Pts',(70.7822037837465,-15.383775718449,-439.937224614613));
#31645=CARTESIAN_POINT('Origin',(52.9999999999906,86.831000000001,-377.5));
#31646=CARTESIAN_POINT('',(53.9999999999878,95.6310000000053,-377.500000000001));
#31647=CARTESIAN_POINT('Origin',(53.9999999999885,86.831000000001,-377.5));
#31648=CARTESIAN_POINT('',(51.9999999999918,95.6310000000052,-377.500000000001));
#31649=CARTESIAN_POINT('',(52.9999999999898,95.6310000000053,-377.500000000001));
#31650=CARTESIAN_POINT('Origin',(51.9999999999926,86.831000000001,-377.5));
#31651=CARTESIAN_POINT('Origin',(52.9999999999906,86.8310000000061,-333.499999999996));
#31652=CARTESIAN_POINT('',(53.9999999999878,95.6310000000105,-333.499999999997));
#31653=CARTESIAN_POINT('Origin',(53.9999999999885,86.8310000000061,-333.499999999997));
#31654=CARTESIAN_POINT('',(51.9999999999918,95.6310000000103,-333.499999999997));
#31655=CARTESIAN_POINT('',(52.9999999999898,95.6310000000104,-333.499999999997));
#31656=CARTESIAN_POINT('Origin',(51.9999999999926,86.8310000000061,-333.499999999996));
#31657=CARTESIAN_POINT('Origin',(1.11022302462516E-13,4.46745505172652E-11,
41.4999999999416));
#31658=CARTESIAN_POINT('',(-4.42323460632396E-13,6.34999999994952,41.4999999999768));
#31659=CARTESIAN_POINT('',(-4.42323460635528E-13,6.34999999998547,41.4999999999408));
#31660=CARTESIAN_POINT('Origin',(1.11022302462516E-13,4.46745505172735E-11,
41.5000000000134));
#31661=CARTESIAN_POINT('Origin',(1.11022302462516E-13,4.52574176051934E-11,
46.6250000000134));
#31662=CARTESIAN_POINT('',(-3.68253555343357E-13,5.50000000004467,41.5000000000128));
#31663=CARTESIAN_POINT('Origin',(1.10718178859001E-13,4.46664927267193E-11,
41.5000000000134));
#31664=CARTESIAN_POINT('',(-3.68253555343282E-13,5.5000000000438,34.0000000000128));
#31665=CARTESIAN_POINT('',(-3.68253555343408E-13,5.50000000004526,46.6250000000128));
#31666=CARTESIAN_POINT('',(5.90298160273389E-13,-5.50000000001298,34.000000000014));
#31667=CARTESIAN_POINT('Origin',(1.11022302462516E-13,4.38141276731807E-11,
34.0000000000134));
#31668=CARTESIAN_POINT('Origin',(1.11022302462516E-13,4.38141276731807E-11,
34.0000000000134));
#31669=CARTESIAN_POINT('Origin',(125.,-11.169000000001,-461.499999999986));
#31670=CARTESIAN_POINT('',(-52.1061868616723,-40.3862650211908,-461.499999999981));
#31671=CARTESIAN_POINT('',(-52.1061868616775,18.0482650211561,-461.499999999988));
#31672=CARTESIAN_POINT('Origin',(125.000000000001,-11.1690000000008,-461.499999999987));
#31673=CARTESIAN_POINT('',(-52.1061868616723,-40.3862650211909,-462.499999999981));
#31674=CARTESIAN_POINT('',(-52.1061868616723,-40.3862650211908,-461.499999999982));
#31675=CARTESIAN_POINT('',(-52.1061868616775,18.0482650211559,-462.499999999988));
#31676=CARTESIAN_POINT('Origin',(125.000000000005,-11.1690000000027,-462.499999998938));
#31677=CARTESIAN_POINT('',(-52.1061868616775,18.0482650211561,-461.499999999988));
#31678=CARTESIAN_POINT('Origin',(1.11022302462516E-13,4.38141276731807E-11,
33.9999999998916));
#31679=CARTESIAN_POINT('',(1.11022302462543E-13,4.34973671664388E-11,31.2499999996439));
#31680=CARTESIAN_POINT('',(5.9164527173117E-13,-5.49999999976929,33.9999999998922));
#31681=CARTESIAN_POINT('Ctrl Pts',(-69.7885335814896,32.039936012842,-440.9823476426));
#31682=CARTESIAN_POINT('Ctrl Pts',(-69.7776904941909,32.0305578312519,-441.000027286454));
#31683=CARTESIAN_POINT('Ctrl Pts',(-69.5538754530634,37.1252327578524,-440.982079016193));
#31684=CARTESIAN_POINT('Ctrl Pts',(-69.5425906598027,37.113747189771,-440.99999999999));
#31685=CARTESIAN_POINT('Ctrl Pts',(-67.6435743056599,41.8415378856266,-440.982079016193));
#31686=CARTESIAN_POINT('Ctrl Pts',(-67.6327997693356,41.8281639590277,-440.99999999999));
#31687=CARTESIAN_POINT('Ctrl Pts',(-64.2753290142128,45.652151355614,-440.981957227449));
#31688=CARTESIAN_POINT('Ctrl Pts',(-64.2658958771893,45.637476314079,-440.999637204013));
#31689=CARTESIAN_POINT('',(-69.7776905149964,32.0305573814079,-441.000027286453));
#31690=CARTESIAN_POINT('',(-66.07358548387,43.2921573753126,-440.999810981737));
#31691=CARTESIAN_POINT('Origin',(-47.744837071413,30.9950012145811,-440.998278175537));
#31692=CARTESIAN_POINT('Ctrl Pts',(-66.07358548387,43.2921573753126,-440.999810981737));
#31693=CARTESIAN_POINT('Ctrl Pts',(-67.1868327014352,41.6282336258689,-440.99958021146));
#31694=CARTESIAN_POINT('Ctrl Pts',(-68.0685532114393,39.8205645108678,-440.999180312587));
#31695=CARTESIAN_POINT('Ctrl Pts',(-69.0695679316239,36.7792652847884,-440.998939961127));
#31696=CARTESIAN_POINT('Ctrl Pts',(-69.351131410688,35.6109067469029,-440.998942059551));
#31697=CARTESIAN_POINT('Ctrl Pts',(-69.6602915252648,33.6321769872792,-440.999335940571));
#31698=CARTESIAN_POINT('Ctrl Pts',(-69.7408627779659,32.8326707807528,-440.99959902782));
#31699=CARTESIAN_POINT('Ctrl Pts',(-69.7776892840197,32.0305577767104,-441.000029187691));
#31700=CARTESIAN_POINT('Ctrl Pts',(64.2809593455634,45.6547550552671,-440.98049740866));
#31701=CARTESIAN_POINT('Ctrl Pts',(64.2705054959308,45.6385004273605,-441.000078147052));
#31702=CARTESIAN_POINT('Ctrl Pts',(67.6447335076994,41.8429767487719,-440.980150947971));
#31703=CARTESIAN_POINT('Ctrl Pts',(67.6327997693276,41.8281639590396,-440.999999999992));
#31704=CARTESIAN_POINT('Ctrl Pts',(69.5550895522119,37.1264684578182,-440.980150947971));
#31705=CARTESIAN_POINT('Ctrl Pts',(69.5425906597955,37.1137471897833,-440.999999999992));
#31706=CARTESIAN_POINT('Ctrl Pts',(69.7936785182884,32.0432074888088,-440.980518645148));
#31707=CARTESIAN_POINT('Ctrl Pts',(69.7816652336223,32.0328182762799,-441.000100325617));
#31708=CARTESIAN_POINT('Origin',(47.8350487511125,31.0311022099888,-441.00118582651));
#31709=CARTESIAN_POINT('Ctrl Pts',(69.7816652336224,32.0328182762799,-441.000100325617));
#31710=CARTESIAN_POINT('Ctrl Pts',(69.7518843882855,32.6817941814599,-440.998904011986));
#31711=CARTESIAN_POINT('Ctrl Pts',(69.6934625136204,33.3291394297202,-440.997957204299));
#31712=CARTESIAN_POINT('Ctrl Pts',(69.5231554244232,34.5910307977996,-440.99650408746));
#31713=CARTESIAN_POINT('Ctrl Pts',(69.4135787649794,35.2052865159601,-440.995982544645));
#31714=CARTESIAN_POINT('Ctrl Pts',(69.1056439599675,36.589400265789,-440.995153783906));
#31715=CARTESIAN_POINT('Ctrl Pts',(68.8914233630438,37.3548496771541,-440.994944699506));
#31716=CARTESIAN_POINT('Ctrl Pts',(68.2710180729107,39.1849139644065,-440.994911067285));
#31717=CARTESIAN_POINT('Ctrl Pts',(67.8228059244791,40.2328726275071,-440.995291719939));
#31718=CARTESIAN_POINT('Ctrl Pts',(66.4689261490073,42.8241873584825,-440.996896227121));
#31719=CARTESIAN_POINT('Ctrl Pts',(65.4530647309365,44.3006265039595,-440.998470978792));
#31720=CARTESIAN_POINT('Ctrl Pts',(64.270505495931,45.6385004273601,-441.000078147052));
#31721=CARTESIAN_POINT('Ctrl Pts',(64.2705054959308,45.6385004273605,-441.000078147052));
#31722=CARTESIAN_POINT('Ctrl Pts',(52.7925979348309,27.7915710081813,-462.498943458995));
#31723=CARTESIAN_POINT('Ctrl Pts',(67.6327997693276,41.8281639590396,-440.999999999992));
#31724=CARTESIAN_POINT('Ctrl Pts',(54.7064708585553,25.7833181444813,-462.499999999991));
#31725=CARTESIAN_POINT('Ctrl Pts',(69.5425906597955,37.1137471897833,-440.999999999992));
#31726=CARTESIAN_POINT('Ctrl Pts',(56.0041009291211,23.3343857139696,-462.49999999999));
#31727=CARTESIAN_POINT('Ctrl Pts',(69.7816652336223,32.0328182762799,-441.000100325617));
#31728=CARTESIAN_POINT('Ctrl Pts',(56.5915605594642,20.6258796622937,-462.49999999999));
#31729=CARTESIAN_POINT('',(56.5915605594642,20.6258796622937,-462.49999999999));
#31730=CARTESIAN_POINT('',(69.7816652336224,32.0328182762798,-441.000100325617));
#31731=CARTESIAN_POINT('',(53.0296962895253,27.5362761699812,-462.499535472188));
#31732=CARTESIAN_POINT('Ctrl Pts',(53.0300419063622,27.5365540887963,-462.4990707585));
#31733=CARTESIAN_POINT('Ctrl Pts',(53.2015496317819,27.3480106076271,-462.49915996944));
#31734=CARTESIAN_POINT('Ctrl Pts',(53.3687845536093,27.1545069130794,-462.499240999659));
#31735=CARTESIAN_POINT('Ctrl Pts',(53.5313403519166,26.9563420647616,-462.499314432669));
#31736=CARTESIAN_POINT('Ctrl Pts',(53.6934013451948,26.7587804121745,-462.499387642156));
#31737=CARTESIAN_POINT('Ctrl Pts',(53.850811280172,26.5565861676637,-462.49945330107));
#31738=CARTESIAN_POINT('Ctrl Pts',(54.0031963229347,26.3500987421599,-462.49951205977));
#31739=CARTESIAN_POINT('Ctrl Pts',(54.1597252568381,26.1379961893595,-462.499572416329));
#31740=CARTESIAN_POINT('Ctrl Pts',(54.3109517332303,25.9213638896764,-462.499625492546));
#31741=CARTESIAN_POINT('Ctrl Pts',(54.4565083889137,25.7006130098379,-462.499672064642));
#31742=CARTESIAN_POINT('Ctrl Pts',(54.5976460796388,25.4865639218063,-462.499717222852));
#31743=CARTESIAN_POINT('Ctrl Pts',(54.7334528676258,25.2686430436956,-462.499756266788));
#31744=CARTESIAN_POINT('Ctrl Pts',(54.8636333433693,25.0472601517917,-462.499789960424));
#31745=CARTESIAN_POINT('Ctrl Pts',(54.9937540045974,24.825978979522,-462.499823638579));
#31746=CARTESIAN_POINT('Ctrl Pts',(55.1182532692508,24.6012393380423,-462.499851972027));
#31747=CARTESIAN_POINT('Ctrl Pts',(55.236879250096,24.3734796429302,-462.499875769413));
#31748=CARTESIAN_POINT('Ctrl Pts',(55.3555307652856,24.1456709223478,-462.49989957192));
#31749=CARTESIAN_POINT('Ctrl Pts',(55.4683062680139,23.9148412445512,-462.499918837139));
#31750=CARTESIAN_POINT('Ctrl Pts',(55.5750002656745,23.6814528220458,-462.499934409438));
#31751=CARTESIAN_POINT('Ctrl Pts',(55.6817890000358,23.4478571671789,-462.499949995564));
#31752=CARTESIAN_POINT('Ctrl Pts',(55.7824852825477,23.2116986428949,-462.499961882973));
#31753=CARTESIAN_POINT('Ctrl Pts',(55.8769322876267,22.9734581004061,-462.499970942341));
#31754=CARTESIAN_POINT('Ctrl Pts',(55.971639256022,22.7345618060333,-462.499980026645));
#31755=CARTESIAN_POINT('Ctrl Pts',(56.0600624058537,22.4935724529541,-462.499986268102));
#31756=CARTESIAN_POINT('Ctrl Pts',(56.1420948629952,22.2509859138938,-462.499990557135));
#31757=CARTESIAN_POINT('Ctrl Pts',(56.2242902121949,22.0079176701276,-462.499994854686));
#31758=CARTESIAN_POINT('Ctrl Pts',(56.3000694465316,21.7632463371213,-462.499997192841));
#31759=CARTESIAN_POINT('Ctrl Pts',(56.3693772469459,21.5174751624493,-462.499998468048));
#31760=CARTESIAN_POINT('Ctrl Pts',(56.4389505167557,21.2707626114129,-462.49999974814));
#31761=CARTESIAN_POINT('Ctrl Pts',(56.5020027183568,21.0229422220262,-462.499999957906));
#31762=CARTESIAN_POINT('Ctrl Pts',(56.5585303196142,20.7745207724168,-462.499999992997));
#31763=CARTESIAN_POINT('Ctrl Pts',(56.5697994701431,20.724996316258,-462.499999999993));
#31764=CARTESIAN_POINT('Ctrl Pts',(56.580809477877,20.6754479526699,-462.49999999999));
#31765=CARTESIAN_POINT('Ctrl Pts',(56.5915605594642,20.6258796622937,-462.49999999999));
#31766=CARTESIAN_POINT('Ctrl Pts',(53.030005423924,27.5365939049776,-462.499070944381));
#31767=CARTESIAN_POINT('Ctrl Pts',(53.5773086193955,28.4845508466792,-461.404278299304));
#31768=CARTESIAN_POINT('Ctrl Pts',(54.1393619772859,29.4580558191063,-460.280364313678));
#31769=CARTESIAN_POINT('Ctrl Pts',(55.3016968424015,31.4712788608959,-457.956521108394));
#31770=CARTESIAN_POINT('Ctrl Pts',(55.9376439432745,32.5727715505385,-456.685346754008));
#31771=CARTESIAN_POINT('Ctrl Pts',(56.5529890060882,33.6385804635187,-455.455487085885));
#31772=CARTESIAN_POINT('Ctrl Pts',(57.8778422943977,15.3629606180432,-462.504468150655));
#31773=CARTESIAN_POINT('Ctrl Pts',(57.8804420169269,15.3637472976184,-462.499999999989));
#31774=CARTESIAN_POINT('Ctrl Pts',(71.5535162631277,19.501120323523,-438.999979560409));
#31775=CARTESIAN_POINT('Ctrl Pts',(57.875348319425,15.354802038958,-462.504468081353));
#31776=CARTESIAN_POINT('Ctrl Pts',(57.8779477730967,15.3555885117513,-462.499999999989));
#31777=CARTESIAN_POINT('Ctrl Pts',(71.5498292133137,19.4919801773738,-438.999986373603));
#31778=CARTESIAN_POINT('Ctrl Pts',(57.8728543444523,15.3466434598728,-462.504468012053));
#31779=CARTESIAN_POINT('Ctrl Pts',(57.8754535292664,15.3474297258841,-462.499999999989));
#31780=CARTESIAN_POINT('Ctrl Pts',(71.5461421634996,19.4828400312246,-438.999993186796));
#31781=CARTESIAN_POINT('Ctrl Pts',(57.8703603694796,15.3384848807876,-462.504467942754));
#31782=CARTESIAN_POINT('Ctrl Pts',(57.8729592854362,15.3392709400169,-462.499999999989));
#31783=CARTESIAN_POINT('Ctrl Pts',(71.5424551136857,19.4736998850754,-438.99999999999));
#31784=CARTESIAN_POINT('',(64.5871672591961,17.3700458363661,-450.95723971308));
#31785=CARTESIAN_POINT('',(65.2503505017821,17.5706789545087,-449.81715836622));
#31786=CARTESIAN_POINT('',(64.5871632769409,17.3700261100896,-450.957233845127));
#31787=CARTESIAN_POINT('Ctrl Pts',(65.2503505017068,17.5706789550751,-449.817158366273));
#31788=CARTESIAN_POINT('Ctrl Pts',(65.1399402715371,17.5378213168938,-450.007344522965));
#31789=CARTESIAN_POINT('Ctrl Pts',(65.0294703630796,17.5046773948113,-450.197443704583));
#31790=CARTESIAN_POINT('Ctrl Pts',(64.808407856047,17.4378034358709,-450.577473377674));
#31791=CARTESIAN_POINT('Ctrl Pts',(64.6978178839098,17.4040741936062,-450.767399354003));
#31792=CARTESIAN_POINT('Ctrl Pts',(64.58716725919,17.3700458364086,-450.957239713085));
#31793=CARTESIAN_POINT('Ctrl Pts',(58.315252633502,-29.4505673778293,-462.499999999984));
#31794=CARTESIAN_POINT('Ctrl Pts',(70.9913620171487,-32.1584685094449,-439.002497203513));
#31795=CARTESIAN_POINT('Ctrl Pts',(57.2363227370075,-31.9735001917283,-462.499999999984));
#31796=CARTESIAN_POINT('Ctrl Pts',(70.1312984392538,-35.2664311746943,-438.996844362179));
#31797=CARTESIAN_POINT('Ctrl Pts',(57.0028527821642,-34.8311127366432,-462.499999999984));
#31798=CARTESIAN_POINT('Ctrl Pts',(70.2493774551285,-38.6061780586552,-439.002389441109));
#31799=CARTESIAN_POINT('Ctrl Pts',(57.872959299689,-37.6772709866423,-462.499999999983));
#31800=CARTESIAN_POINT('Ctrl Pts',(71.5424551348726,-41.8116999372577,-438.999999999983));
#31801=CARTESIAN_POINT('',(64.5798198703728,-39.7058474679734,-450.969887422476));
#31802=CARTESIAN_POINT('',(65.2610173681319,-39.9118525359211,-449.798783660325));
#31803=CARTESIAN_POINT('',(64.5798106827944,-39.7058023136291,-450.96987413409));
#31804=CARTESIAN_POINT('',(57.7295804999108,-37.1684431732989,-462.499999999983));
#31805=CARTESIAN_POINT('Ctrl Pts',(57.729580499911,-37.1684431732993,-462.499999999983));
#31806=CARTESIAN_POINT('Ctrl Pts',(58.8199723157923,-37.6567760006761,-460.693530021075));
#31807=CARTESIAN_POINT('Ctrl Pts',(59.923205364492,-38.1000146374347,-458.856471844879));
#31808=CARTESIAN_POINT('Ctrl Pts',(62.2046437952623,-38.9433259685703,-455.022540409383));
#31809=CARTESIAN_POINT('Ctrl Pts',(63.3997482388661,-39.3427460598765,-452.994373238536));
#31810=CARTESIAN_POINT('Ctrl Pts',(64.5798065713121,-39.705781792052,-450.969867971454));
#31811=CARTESIAN_POINT('',(58.315252633502,-29.4505673778293,-462.499999999984));
#31812=CARTESIAN_POINT('Ctrl Pts',(58.3152526334998,-29.4505673778284,-462.499999999988));
#31813=CARTESIAN_POINT('Ctrl Pts',(57.7976276531132,-30.6609639499824,-462.499999999988));
#31814=CARTESIAN_POINT('Ctrl Pts',(57.4826884205137,-31.9483301287851,-462.499999999987));
#31815=CARTESIAN_POINT('Ctrl Pts',(57.2834655596958,-34.5736510331327,-462.499999999987));
#31816=CARTESIAN_POINT('Ctrl Pts',(57.4005339681898,-35.8938034717833,-462.499999999988));
#31817=CARTESIAN_POINT('Ctrl Pts',(57.7295829994487,-37.1684528558765,-462.499999999988));
#31818=CARTESIAN_POINT('',(58.315252633502,-29.4505673778293,-462.499999999984));
#31819=CARTESIAN_POINT('Ctrl Pts',(70.459364073535,-36.7925280866649,-438.999999999984));
#31820=CARTESIAN_POINT('Ctrl Pts',(70.4453273089361,-36.4542715080457,-438.999999999984));
#31821=CARTESIAN_POINT('Ctrl Pts',(70.4427173721536,-36.1156409498122,-438.999999999982));
#31822=CARTESIAN_POINT('Ctrl Pts',(70.4603981657122,-35.4387755921454,-438.999999999983));
#31823=CARTESIAN_POINT('Ctrl Pts',(70.4806827099488,-35.1007537261475,-438.999999999984));
#31824=CARTESIAN_POINT('Ctrl Pts',(70.5123942581111,-34.7636934497019,-438.999999999984));
#31825=CARTESIAN_POINT('Ctrl Pts',(65.2610173681319,-39.9118525359211,-449.798783660325));
#31826=CARTESIAN_POINT('Ctrl Pts',(66.0967783128156,-40.1604407556788,-448.359058582003));
#31827=CARTESIAN_POINT('Ctrl Pts',(66.9275802964328,-40.392196036837,-446.916923734249));
#31828=CARTESIAN_POINT('Ctrl Pts',(68.5997382095796,-40.8322295918434,-443.993321242625));
#31829=CARTESIAN_POINT('Ctrl Pts',(69.4492098945576,-41.0416415242989,-442.496899945137));
#31830=CARTESIAN_POINT('Ctrl Pts',(70.2929704405245,-41.2369817291983,-441.000070382422));
#31831=CARTESIAN_POINT('Ctrl Pts',(69.7946169307026,-54.38201903755,-440.978989030848));
#31832=CARTESIAN_POINT('Ctrl Pts',(69.7816652336298,-54.3708182762895,-441.000100325607));
#31833=CARTESIAN_POINT('Ctrl Pts',(69.5560658976611,-59.4654621740419,-440.978600448059));
#31834=CARTESIAN_POINT('Ctrl Pts',(69.5425906598038,-59.4517471897933,-440.999999999981));
#31835=CARTESIAN_POINT('Ctrl Pts',(67.6456657063917,-64.182133843286,-440.978600448058));
#31836=CARTESIAN_POINT('Ctrl Pts',(67.6327997693368,-64.1661639590497,-440.99999999998));
#31837=CARTESIAN_POINT('Ctrl Pts',(64.2817759434034,-67.9940247783317,-440.978967867946));
#31838=CARTESIAN_POINT('Ctrl Pts',(64.2705054959406,-67.9765004273711,-441.000078147038));
#31839=CARTESIAN_POINT('',(64.2705054959405,-67.9765004273713,-441.000078147038));
#31840=CARTESIAN_POINT('Origin',(47.8350487510253,-53.3691022099654,-441.001185826503));
#31841=CARTESIAN_POINT('Ctrl Pts',(64.2705054959406,-67.9765004273711,-441.000078147038));
#31842=CARTESIAN_POINT('Ctrl Pts',(65.3713757282322,-66.7310443578283,-440.998581998987));
#31843=CARTESIAN_POINT('Ctrl Pts',(66.3280443259402,-65.3652099283856,-440.997113886392));
#31844=CARTESIAN_POINT('Ctrl Pts',(67.7249250139629,-62.7970659610114,-440.99537830064));
#31845=CARTESIAN_POINT('Ctrl Pts',(68.2314861563532,-61.6395247500074,-440.994908924246));
#31846=CARTESIAN_POINT('Ctrl Pts',(68.9087860162404,-59.6416335258256,-440.994945640725));
#31847=CARTESIAN_POINT('Ctrl Pts',(69.1346111078826,-58.8231493981561,-440.995183026277));
#31848=CARTESIAN_POINT('Ctrl Pts',(69.438858496689,-57.4066076677694,-440.996093834534));
#31849=CARTESIAN_POINT('Ctrl Pts',(69.5409437946101,-56.8146091059414,-440.996619383099));
#31850=CARTESIAN_POINT('Ctrl Pts',(69.6989501274562,-55.6056200152367,-440.998047800919));
#31851=CARTESIAN_POINT('Ctrl Pts',(69.7532997046084,-54.9889520016567,-440.998960866044));
#31852=CARTESIAN_POINT('Ctrl Pts',(69.7816652336299,-54.3708182762896,-441.000100325607));
#31853=CARTESIAN_POINT('Ctrl Pts',(69.7816652336298,-54.3708182762895,-441.000100325607));
#31854=CARTESIAN_POINT('Ctrl Pts',(56.5915605594697,-42.9638796623104,-462.499999999983));
#31855=CARTESIAN_POINT('Ctrl Pts',(69.5425906598038,-59.4517471897933,-440.999999999981));
#31856=CARTESIAN_POINT('Ctrl Pts',(56.0041009291271,-45.6723857139866,-462.499999999983));
#31857=CARTESIAN_POINT('Ctrl Pts',(67.6327997693368,-64.1661639590497,-440.99999999998));
#31858=CARTESIAN_POINT('Ctrl Pts',(54.7064708585618,-48.1213181444985,-462.499999999982));
#31859=CARTESIAN_POINT('Ctrl Pts',(64.2705054959406,-67.9765004273711,-441.000078147038));
#31860=CARTESIAN_POINT('Ctrl Pts',(52.7925979348378,-50.1295710081989,-462.498943458986));
#31861=CARTESIAN_POINT('',(56.5915605594697,-42.9638796623104,-462.499999999983));
#31862=CARTESIAN_POINT('',(69.7816652336299,-54.3708182762896,-441.000100325607));
#31863=CARTESIAN_POINT('',(56.5529890060961,-55.9765804635348,-455.455487085874));
#31864=CARTESIAN_POINT('',(64.2705054959405,-67.9765004273713,-441.000078147038));
#31865=CARTESIAN_POINT('',(53.029696289532,-49.8742761699988,-462.499535472179));
#31866=CARTESIAN_POINT('Ctrl Pts',(56.5529890060963,-55.9765804635346,-455.455487085874));
#31867=CARTESIAN_POINT('Ctrl Pts',(55.9381283183532,-54.9116105127872,-456.684378657559));
#31868=CARTESIAN_POINT('Ctrl Pts',(55.3027200270559,-53.8110510686363,-457.954475902198));
#31869=CARTESIAN_POINT('Ctrl Pts',(54.1403899944375,-51.7978363969789,-460.278308627195));
#31870=CARTESIAN_POINT('Ctrl Pts',(53.5778030008828,-50.8234071405388,-461.40328936809));
#31871=CARTESIAN_POINT('Ctrl Pts',(53.0300054239308,-49.8745939049953,-462.499070944372));
#31872=CARTESIAN_POINT('Ctrl Pts',(56.5915605594697,-42.9638796623104,-462.499999999983));
#31873=CARTESIAN_POINT('Ctrl Pts',(56.537631898305,-43.2125199051099,-462.499999999983));
#31874=CARTESIAN_POINT('Ctrl Pts',(56.4771841693873,-43.4606593871229,-462.500000001674));
#31875=CARTESIAN_POINT('Ctrl Pts',(56.4102105416286,-43.7077927013583,-462.499999113015));
#31876=CARTESIAN_POINT('Ctrl Pts',(56.3434676095377,-43.9540747464168,-462.499998227417));
#31877=CARTESIAN_POINT('Ctrl Pts',(56.2702436069996,-44.1993571047456,-462.499996456823));
#31878=CARTESIAN_POINT('Ctrl Pts',(56.1905834176614,-44.4431360043272,-462.49999290506));
#31879=CARTESIAN_POINT('Ctrl Pts',(56.1089402448685,-44.6929832992829,-462.499989264884));
#31880=CARTESIAN_POINT('Ctrl Pts',(56.0205362191533,-44.9412508502421,-462.499983752903));
#31881=CARTESIAN_POINT('Ctrl Pts',(55.9254766389649,-45.1873997239285,-462.499975402613));
#31882=CARTESIAN_POINT('Ctrl Pts',(55.833195263603,-45.4263546673707,-462.499967296368));
#31883=CARTESIAN_POINT('Ctrl Pts',(55.7346419953777,-45.6633125555955,-462.499956514529));
#31884=CARTESIAN_POINT('Ctrl Pts',(55.6299648435093,-45.8977902129081,-462.499942183297));
#31885=CARTESIAN_POINT('Ctrl Pts',(55.5253792494255,-46.1320627800511,-462.4999278646));
#31886=CARTESIAN_POINT('Ctrl Pts',(55.4146806098435,-46.3638590294524,-462.49991000195));
#31887=CARTESIAN_POINT('Ctrl Pts',(55.2980659547443,-46.5927132907045,-462.499887745806));
#31888=CARTESIAN_POINT('Ctrl Pts',(55.1814748250644,-46.8215213837246,-462.499865494152));
#31889=CARTESIAN_POINT('Ctrl Pts',(55.0589702553333,-47.0473882738389,-462.499838850043));
#31890=CARTESIAN_POINT('Ctrl Pts',(54.9307961809409,-47.2698710119221,-462.499806997694));
#31891=CARTESIAN_POINT('Ctrl Pts',(54.8025614231947,-47.4924590833091,-462.499775130265));
#31892=CARTESIAN_POINT('Ctrl Pts',(54.6686520347203,-47.7116594263157,-462.499738048975));
#31893=CARTESIAN_POINT('Ctrl Pts',(54.529356130181,-47.9270567374448,-462.499694980864));
#31894=CARTESIAN_POINT('Ctrl Pts',(54.389759265441,-48.1429194320911,-462.499651819701));
#31895=CARTESIAN_POINT('Ctrl Pts',(54.2447528711453,-48.3549623037771,-462.499602645179));
#31896=CARTESIAN_POINT('Ctrl Pts',(54.0946669651107,-48.5628011065844,-462.499546733495));
#31897=CARTESIAN_POINT('Ctrl Pts',(53.9443335508868,-48.7709826584683,-462.499490729606));
#31898=CARTESIAN_POINT('Ctrl Pts',(53.7889041971722,-48.9749459760321,-462.49942796576));
#31899=CARTESIAN_POINT('Ctrl Pts',(53.6287459504915,-49.1743434635936,-462.499357777847));
#31900=CARTESIAN_POINT('Ctrl Pts',(53.4680465723631,-49.3744146613969,-462.499287352789));
#31901=CARTESIAN_POINT('Ctrl Pts',(53.3025866634557,-49.5698888785735,-462.499209452928));
#31902=CARTESIAN_POINT('Ctrl Pts',(53.1327672630609,-49.7604578043835,-462.499123478914));
#31903=CARTESIAN_POINT('Ctrl Pts',(53.0986997159057,-49.7986879232701,-462.499106231627));
#31904=CARTESIAN_POINT('Ctrl Pts',(53.0644568094535,-49.8367207747998,-462.499088659643));
#31905=CARTESIAN_POINT('Ctrl Pts',(53.0300419063689,-49.8745540888141,-462.499070758491));
#31906=CARTESIAN_POINT('Ctrl Pts',(56.8171268781939,-75.4544783554495,-440.981517358892));
#31907=CARTESIAN_POINT('Ctrl Pts',(56.8017229870639,-75.4445663251619,-441.000077552423));
#31908=CARTESIAN_POINT('Ctrl Pts',(53.0022604651873,-78.8200388563469,-440.981185782947));
#31909=CARTESIAN_POINT('Ctrl Pts',(52.9882277636123,-78.8087212293983,-440.999999999979));
#31910=CARTESIAN_POINT('Ctrl Pts',(48.2867035759484,-80.7296085197381,-440.981185782946));
#31911=CARTESIAN_POINT('Ctrl Pts',(48.274652617608,-80.7177558649672,-440.999999999978));
#31912=CARTESIAN_POINT('Ctrl Pts',(43.2073677667846,-80.9657191524129,-440.981499301018));
#31913=CARTESIAN_POINT('Ctrl Pts',(43.197523751011,-80.9543288413526,-441.000060412176));
#31914=CARTESIAN_POINT('',(56.8017229870589,-75.4445663251663,-441.000077552423));
#31915=CARTESIAN_POINT('',(43.1975237510109,-80.9543288413527,-441.000060412177));
#31916=CARTESIAN_POINT('Origin',(42.2233532178455,-58.9519567778136,-441.000918028327));
#31917=CARTESIAN_POINT('Ctrl Pts',(43.1975237510113,-80.9543288413526,-441.000060412176));
#31918=CARTESIAN_POINT('Ctrl Pts',(44.4031402145552,-80.8989945191125,-440.998726536663));
#31919=CARTESIAN_POINT('Ctrl Pts',(45.6021895814689,-80.7448684887729,-440.997737499632));
#31920=CARTESIAN_POINT('Ctrl Pts',(47.9449883857747,-80.245975858692,-440.996451146542));
#31921=CARTESIAN_POINT('Ctrl Pts',(49.0854799958832,-79.9049726728867,-440.996144855277));
#31922=CARTESIAN_POINT('Ctrl Pts',(51.4454681110207,-78.9862019845966,-440.996145395842));
#31923=CARTESIAN_POINT('Ctrl Pts',(52.6508252985512,-78.3851936817408,-440.996537734672));
#31924=CARTESIAN_POINT('Ctrl Pts',(54.858065396025,-77.0203018770163,-440.997937064421));
#31925=CARTESIAN_POINT('Ctrl Pts',(55.8642654113312,-76.2730348674113,-440.998896997706));
#31926=CARTESIAN_POINT('Ctrl Pts',(56.8017229870589,-75.4445663251663,-441.000077552423));
#31927=CARTESIAN_POINT('Ctrl Pts',(56.8017229870639,-75.4445663251619,-441.000077552423));
#31928=CARTESIAN_POINT('Ctrl Pts',(38.9588941886819,-63.9631388095498,-462.498954222077));
#31929=CARTESIAN_POINT('Ctrl Pts',(52.9882277636123,-78.8087212293983,-440.999999999979));
#31930=CARTESIAN_POINT('Ctrl Pts',(36.9523181444951,-65.8754708585682,-462.499999999979));
#31931=CARTESIAN_POINT('Ctrl Pts',(48.274652617608,-80.7177558649672,-440.999999999978));
#31932=CARTESIAN_POINT('Ctrl Pts',(34.5033857139835,-67.173100929134,-462.499999999979));
#31933=CARTESIAN_POINT('Ctrl Pts',(43.197523751011,-80.9543288413526,-441.000060412176));
#31934=CARTESIAN_POINT('Ctrl Pts',(31.7948796623075,-67.7605605594772,-462.499999999979));
#31935=CARTESIAN_POINT('',(44.7374479017836,-67.6814979527098,-455.536357931381));
#31936=CARTESIAN_POINT('',(56.8017229870589,-75.4445663251663,-441.000077552423));
#31937=CARTESIAN_POINT('',(31.7948796623075,-67.7605605594772,-462.499999999979));
#31938=CARTESIAN_POINT('',(43.1975237510109,-80.9543288413527,-441.000060412177));
#31939=CARTESIAN_POINT('',(38.7052882157426,-64.1987044759212,-462.499539856792));
#31940=CARTESIAN_POINT('Ctrl Pts',(38.7055635736167,-64.1990467954908,-462.499079528891));
#31941=CARTESIAN_POINT('Ctrl Pts',(38.5172275971445,-64.3704105530215,-462.499167854858));
#31942=CARTESIAN_POINT('Ctrl Pts',(38.3239197960279,-64.5375163457007,-462.499248085453));
#31943=CARTESIAN_POINT('Ctrl Pts',(38.1259398426536,-64.699957188765,-462.49932079767));
#31944=CARTESIAN_POINT('Ctrl Pts',(37.9285425865703,-64.8619199337311,-462.49939329588));
#31945=CARTESIAN_POINT('Ctrl Pts',(37.726500868484,-65.0192447705182,-462.499458320352));
#31946=CARTESIAN_POINT('Ctrl Pts',(37.5201548987088,-65.1715569484135,-462.49951651441));
#31947=CARTESIAN_POINT('Ctrl Pts',(37.3080980013927,-65.3280845893609,-462.499576319074));
#31948=CARTESIAN_POINT('Ctrl Pts',(37.0914954019602,-65.4793177024024,-462.499628910257));
#31949=CARTESIAN_POINT('Ctrl Pts',(36.8707598320672,-65.6248872824809,-462.499675056921));
#31950=CARTESIAN_POINT('Ctrl Pts',(36.6567884437342,-65.7659960542278,-462.499719789474));
#31951=CARTESIAN_POINT('Ctrl Pts',(36.4389340209405,-65.9017829622837,-462.499758467341));
#31952=CARTESIAN_POINT('Ctrl Pts',(36.2176075522289,-66.0319513181425,-462.499791846736));
#31953=CARTESIAN_POINT('Ctrl Pts',(35.9963765196386,-66.1620635453191,-462.499825211738));
#31954=CARTESIAN_POINT('Ctrl Pts',(35.7716767996782,-66.2865618098307,-462.499853283506));
#31955=CARTESIAN_POINT('Ctrl Pts',(35.5439481503633,-66.4051928613635,-462.499876862572));
#31956=CARTESIAN_POINT('Ctrl Pts',(35.316169349663,-66.5238500383382,-462.499900446831));
#31957=CARTESIAN_POINT('Ctrl Pts',(35.0853606833263,-66.6366372165729,-462.49991953713));
#31958=CARTESIAN_POINT('Ctrl Pts',(34.8519857935553,-66.7433474955649,-462.499934969413));
#31959=CARTESIAN_POINT('Ctrl Pts',(34.6184080394107,-66.8501505339532,-462.499950415112));
#31960=CARTESIAN_POINT('Ctrl Pts',(34.3822600211211,-66.9508659603753,-462.499962197189));
#31961=CARTESIAN_POINT('Ctrl Pts',(34.1440240563708,-67.0453355257903,-462.499971177619));
#31962=CARTESIAN_POINT('Ctrl Pts',(33.9051482369425,-67.1400588177718,-462.499980182168));
#31963=CARTESIAN_POINT('Ctrl Pts',(33.664173678481,-67.2285025608647,-462.499986370777));
#31964=CARTESIAN_POINT('Ctrl Pts',(33.4215976713632,-67.3105584616105,-462.499990624821));
#31965=CARTESIAN_POINT('Ctrl Pts',(33.1785544871469,-67.3927723938042,-462.499994887057));
#31966=CARTESIAN_POINT('Ctrl Pts',(32.9339041272313,-67.4685738375367,-462.49999720805));
#31967=CARTESIAN_POINT('Ctrl Pts',(32.6881511913545,-67.5379060565884,-462.499998475006));
#31968=CARTESIAN_POINT('Ctrl Pts',(32.4414818006612,-67.6074968273676,-462.499999746687));
#31969=CARTESIAN_POINT('Ctrl Pts',(32.1937020411489,-67.6705700690391,-462.499999957227));
#31970=CARTESIAN_POINT('Ctrl Pts',(31.9453199033596,-67.7271208240112,-462.499999992803));
#31971=CARTESIAN_POINT('Ctrl Pts',(31.8951963275913,-67.7385327801076,-462.499999999982));
#31972=CARTESIAN_POINT('Ctrl Pts',(31.8450482010303,-67.7496792874214,-462.499999999979));
#31973=CARTESIAN_POINT('Ctrl Pts',(31.7948796623075,-67.7605605594772,-462.499999999979));
#31974=CARTESIAN_POINT('Ctrl Pts',(38.7056029900764,-64.1990106692133,-462.4990797136));
#31975=CARTESIAN_POINT('Ctrl Pts',(39.6432579745448,-64.7403660269029,-461.416170705934));
#31976=CARTESIAN_POINT('Ctrl Pts',(40.6056781462348,-65.296019572104,-460.305037237873));
#31977=CARTESIAN_POINT('Ctrl Pts',(42.5961675836127,-66.4452291845927,-458.007400411776));
#31978=CARTESIAN_POINT('Ctrl Pts',(43.6839808596153,-67.0732784723181,-456.751993534114));
#31979=CARTESIAN_POINT('Ctrl Pts',(44.7374479017911,-67.6814979527005,-455.536357931383));
#31980=CARTESIAN_POINT('Ctrl Pts',(-43.2047136373585,-80.966056949464,-440.981137741313));
#31981=CARTESIAN_POINT('Ctrl Pts',(-43.1946805031653,-80.9544448157854,
-441.000060157993));
#31982=CARTESIAN_POINT('Ctrl Pts',(-48.2869381564542,-80.7298392401449,
-440.980819550762));
#31983=CARTESIAN_POINT('Ctrl Pts',(-48.2746526175946,-80.7177558649757,
-440.999999999976));
#31984=CARTESIAN_POINT('Ctrl Pts',(-53.0025336217422,-78.8202591620554,
-440.980819550762));
#31985=CARTESIAN_POINT('Ctrl Pts',(-52.9882277635993,-78.8087212294075,
-440.999999999977));
#31986=CARTESIAN_POINT('Ctrl Pts',(-56.8142200441329,-75.4551560531967,
-440.98112498298));
#31987=CARTESIAN_POINT('Ctrl Pts',(-56.7985201760894,-75.4450502563038,
-441.000046863259));
#31988=CARTESIAN_POINT('',(-43.1946805031654,-80.9544448157855,-441.000060157993));
#31989=CARTESIAN_POINT('',(-56.7985201761028,-75.4450502562919,-441.000046863259));
#31990=CARTESIAN_POINT('Origin',(-42.1888478026556,-58.9666575781096,-441.000711744184));
#31991=CARTESIAN_POINT('Ctrl Pts',(-56.7985201760894,-75.4450502563038,
-441.000046863259));
#31992=CARTESIAN_POINT('Ctrl Pts',(-56.4263535406146,-75.7739272521541,
-440.99977882747));
#31993=CARTESIAN_POINT('Ctrl Pts',(-56.0431930051001,-76.090149626701,-440.999512160104));
#31994=CARTESIAN_POINT('Ctrl Pts',(-53.724908457157,-77.8754202087466,-440.997991790387));
#31995=CARTESIAN_POINT('Ctrl Pts',(-51.5685554398738,-79.0297799655311,
-440.996935620165));
#31996=CARTESIAN_POINT('Ctrl Pts',(-48.2083577710306,-80.1686711508664,
-440.996972642525));
#31997=CARTESIAN_POINT('Ctrl Pts',(-47.123200326989,-80.4466850673039,-440.997215533442));
#31998=CARTESIAN_POINT('Ctrl Pts',(-45.087048397782,-80.8063142609533,-440.998282797664));
#31999=CARTESIAN_POINT('Ctrl Pts',(-44.1427605555334,-80.9109332077313,
-440.999012122082));
#32000=CARTESIAN_POINT('Ctrl Pts',(-43.1946805031653,-80.9544448157854,
-441.000060157993));
#32001=CARTESIAN_POINT('Ctrl Pts',(-64.2743506444738,-67.9925839239085,
-440.983888214158));
#32002=CARTESIAN_POINT('Ctrl Pts',(-64.2657293397397,-67.9791674266158,
-441.000046512357));
#32003=CARTESIAN_POINT('Ctrl Pts',(-67.6426474509325,-64.1783874243697,
-440.983620627614));
#32004=CARTESIAN_POINT('Ctrl Pts',(-67.6327997693264,-64.1661639590615,
-440.999999999978));
#32005=CARTESIAN_POINT('Ctrl Pts',(-69.552904704657,-59.4622447382962,-440.983620627615));
#32006=CARTESIAN_POINT('Ctrl Pts',(-69.5425906597941,-59.4517471898053,
-440.999999999979));
#32007=CARTESIAN_POINT('Ctrl Pts',(-69.7876243621201,-54.3811153516783,
-440.983874019661));
#32008=CARTESIAN_POINT('Ctrl Pts',(-69.7777140088065,-54.3725409130246,
-441.000032808645));
#32009=CARTESIAN_POINT('',(-64.2657293397398,-67.9791674266157,-441.000046512357));
#32010=CARTESIAN_POINT('',(-69.7777140088065,-54.3725409130246,-441.000032808645));
#32011=CARTESIAN_POINT('Origin',(-47.7498816680565,-53.384540451435,-441.000527747256));
#32012=CARTESIAN_POINT('Ctrl Pts',(-69.7777140088065,-54.3725409130246,
-441.000032808645));
#32013=CARTESIAN_POINT('Ctrl Pts',(-69.7165990727465,-55.7037291462961,
-440.999228486668));
#32014=CARTESIAN_POINT('Ctrl Pts',(-69.535056842701,-57.026651696731,-440.99862757642));
#32015=CARTESIAN_POINT('Ctrl Pts',(-68.9483190906072,-59.5682977466865,
-440.997891639565));
#32016=CARTESIAN_POINT('Ctrl Pts',(-68.5540700559461,-60.7842796997571,
-440.997738224173));
#32017=CARTESIAN_POINT('Ctrl Pts',(-67.6191319824325,-62.9944922976845,
-440.997830589012));
#32018=CARTESIAN_POINT('Ctrl Pts',(-67.1028440820214,-63.9946589547973,
-440.998030525737));
#32019=CARTESIAN_POINT('Ctrl Pts',(-65.8514110837686,-66.0227249818099,
-440.99876113321));
#32020=CARTESIAN_POINT('Ctrl Pts',(-65.0996976290768,-67.0357638306388,
-440.999327438968));
#32021=CARTESIAN_POINT('Ctrl Pts',(-64.2657293397398,-67.9791674266157,
-441.000046512357));
#32022=CARTESIAN_POINT('Origin',(45.9999999999903,112.830999999998,-401.5));
#32023=CARTESIAN_POINT('',(49.9999999999903,112.830999999998,-399.1905989232));
#32024=CARTESIAN_POINT('',(45.9999999999903,112.830999999998,-396.8811978465));
#32025=CARTESIAN_POINT('',(47.9999999999903,112.830999999998,-398.03589838485));
#32026=CARTESIAN_POINT('',(49.9999999999903,112.830999999998,-403.8094010768));
#32027=CARTESIAN_POINT('',(49.9999999999903,112.830999999998,-401.5));
#32028=CARTESIAN_POINT('',(45.9999999999903,112.830999999997,-406.118802153499));
#32029=CARTESIAN_POINT('',(47.9999999999903,112.830999999997,-404.96410161515));
#32030=CARTESIAN_POINT('',(41.9999999999903,112.830999999997,-403.8094010768));
#32031=CARTESIAN_POINT('',(43.9999999999903,112.830999999997,-404.96410161515));
#32032=CARTESIAN_POINT('',(41.9999999999903,112.830999999998,-399.1905989232));
#32033=CARTESIAN_POINT('',(41.9999999999903,112.830999999997,-401.5));
#32034=CARTESIAN_POINT('',(43.9999999999903,112.830999999998,-398.03589838485));
#32035=CARTESIAN_POINT('Origin',(-49.0000000000097,112.830999999989,-401.5));
#32036=CARTESIAN_POINT('',(-45.0000000000097,112.83099999999,-399.1905989232));
#32037=CARTESIAN_POINT('',(-49.0000000000097,112.83099999999,-396.8811978465));
#32038=CARTESIAN_POINT('',(-47.0000000000097,112.83099999999,-398.03589838485));
#32039=CARTESIAN_POINT('',(-45.0000000000097,112.830999999989,-403.8094010768));
#32040=CARTESIAN_POINT('',(-45.0000000000097,112.83099999999,-401.5));
#32041=CARTESIAN_POINT('',(-49.0000000000097,112.830999999989,-406.118802153499));
#32042=CARTESIAN_POINT('',(-47.0000000000097,112.830999999989,-404.96410161515));
#32043=CARTESIAN_POINT('',(-53.0000000000097,112.830999999989,-403.8094010768));
#32044=CARTESIAN_POINT('',(-51.0000000000097,112.830999999989,-404.96410161515));
#32045=CARTESIAN_POINT('',(-53.0000000000097,112.830999999989,-399.1905989232));
#32046=CARTESIAN_POINT('',(-53.0000000000097,112.830999999989,-401.5));
#32047=CARTESIAN_POINT('',(-51.0000000000097,112.83099999999,-398.03589838485));
#32048=CARTESIAN_POINT('Origin',(45.9999999999903,112.831000000008,-309.5));
#32049=CARTESIAN_POINT('',(49.9999999999903,112.831000000009,-307.1905989232));
#32050=CARTESIAN_POINT('',(45.9999999999903,112.831000000009,-304.881197846499));
#32051=CARTESIAN_POINT('',(47.9999999999903,112.831000000009,-306.035898384849));
#32052=CARTESIAN_POINT('',(49.9999999999903,112.831000000008,-311.809401076799));
#32053=CARTESIAN_POINT('',(49.9999999999903,112.831000000009,-309.5));
#32054=CARTESIAN_POINT('',(45.9999999999903,112.831000000008,-314.118802153499));
#32055=CARTESIAN_POINT('',(47.9999999999903,112.831000000008,-312.96410161515));
#32056=CARTESIAN_POINT('',(41.9999999999903,112.831000000008,-311.809401076799));
#32057=CARTESIAN_POINT('',(43.9999999999903,112.831000000008,-312.96410161515));
#32058=CARTESIAN_POINT('',(41.9999999999903,112.831000000008,-307.1905989232));
#32059=CARTESIAN_POINT('',(41.9999999999903,112.831000000008,-309.5));
#32060=CARTESIAN_POINT('',(43.9999999999903,112.831000000008,-306.035898384849));
#32061=CARTESIAN_POINT('Origin',(-49.0000000000097,112.831,-309.5));
#32062=CARTESIAN_POINT('',(-45.0000000000097,112.831,-307.1905989232));
#32063=CARTESIAN_POINT('',(-49.0000000000097,112.831,-304.881197846499));
#32064=CARTESIAN_POINT('',(-47.0000000000097,112.831,-306.035898384849));
#32065=CARTESIAN_POINT('',(-45.0000000000097,112.831,-311.809401076799));
#32066=CARTESIAN_POINT('',(-45.0000000000097,112.831,-309.5));
#32067=CARTESIAN_POINT('',(-49.0000000000097,112.831,-314.118802153499));
#32068=CARTESIAN_POINT('',(-47.0000000000097,112.831,-312.96410161515));
#32069=CARTESIAN_POINT('',(-53.0000000000097,112.831,-311.809401076799));
#32070=CARTESIAN_POINT('',(-51.0000000000097,112.831,-312.96410161515));
#32071=CARTESIAN_POINT('',(-53.0000000000097,112.831,-307.1905989232));
#32072=CARTESIAN_POINT('',(-53.0000000000097,112.831,-309.5));
#32073=CARTESIAN_POINT('',(-51.0000000000097,112.831,-306.035898384849));
#32074=CARTESIAN_POINT('Origin',(26.6129405624652,-47.4885629631521,-461.499999999981));
#32075=CARTESIAN_POINT('',(52.1061868616782,-40.3862650211815,-461.499999999983));
#32076=CARTESIAN_POINT('',(47.6332714621302,-49.0956490614551,-461.499999999982));
#32077=CARTESIAN_POINT('Origin',(36.3195629631445,-37.7819405624712,-461.500000000005));
#32078=CARTESIAN_POINT('',(37.9266490614509,-58.802271462136,-461.49999999998));
#32079=CARTESIAN_POINT('',(47.6332714621302,-49.0956490614551,-461.499999999982));
#32080=CARTESIAN_POINT('',(29.2172650211785,-63.2751868616856,-461.499999999979));
#32081=CARTESIAN_POINT('Origin',(26.6129405624651,-47.488562963152,-461.499999999982));
#32082=CARTESIAN_POINT('',(-29.2172650211685,-63.2751868616907,-461.499999999979));
#32083=CARTESIAN_POINT('Origin',(-1.19904086659517E-11,113.830999999992,
-461.500000000043));
#32084=CARTESIAN_POINT('',(-37.9266490614418,-58.8022714621425,-461.49999999998));
#32085=CARTESIAN_POINT('Origin',(-26.612940562458,-47.4885629631569,-461.499999999995));
#32086=CARTESIAN_POINT('',(-47.6332714621227,-49.0956490614631,-461.49999999998));
#32087=CARTESIAN_POINT('',(-37.9266490614418,-58.8022714621425,-461.49999999998));
#32088=CARTESIAN_POINT('Origin',(-36.3195629631389,-37.7819405624775,-461.499999999979));
#32089=CARTESIAN_POINT('',(-47.6332714621292,26.7576490614296,-461.499999999989));
#32090=CARTESIAN_POINT('Origin',(-36.3195629631435,15.4439405624457,-461.49999999999));
#32091=CARTESIAN_POINT('',(-37.9266490614499,36.4642714621104,-461.49999999999));
#32092=CARTESIAN_POINT('',(-47.6332714621292,26.7576490614295,-461.499999999989));
#32093=CARTESIAN_POINT('',(-29.2172650211774,40.93718686166,-461.499999999991));
#32094=CARTESIAN_POINT('Origin',(-26.6129405624642,25.1505629631267,-461.499999999994));
#32095=CARTESIAN_POINT('',(29.2172650211694,40.9371868616653,-461.499999999991));
#32096=CARTESIAN_POINT('Origin',(1.30295774170008E-11,-136.169000000019,
-461.500000000151));
#32097=CARTESIAN_POINT('',(37.9266490614429,36.4642714621169,-461.499999999991));
#32098=CARTESIAN_POINT('Origin',(26.6129405624589,25.1505629631313,-461.49999999999));
#32099=CARTESIAN_POINT('',(47.6332714621237,26.7576490614377,-461.49999999999));
#32100=CARTESIAN_POINT('',(37.9266490614429,36.4642714621169,-461.499999999991));
#32101=CARTESIAN_POINT('',(52.1061868616731,18.0482650211652,-461.499999999989));
#32102=CARTESIAN_POINT('Origin',(36.31956296314,15.4439405624519,-461.499999999992));
#32103=CARTESIAN_POINT('Origin',(-125.,-11.1690000000242,-461.500000000023));
#32104=CARTESIAN_POINT('Origin',(52.4999999999926,86.8310000000061,-333.499999999996));
#32105=CARTESIAN_POINT('',(52.4999999999928,83.9442486541067,-328.499999999996));
#32106=CARTESIAN_POINT('',(52.4999999999931,81.0574973081061,-333.499999999996));
#32107=CARTESIAN_POINT('',(52.4999999999929,82.5008729811064,-330.999999999996));
#32108=CARTESIAN_POINT('',(52.4999999999928,83.9442486541055,-338.499999999996));
#32109=CARTESIAN_POINT('',(52.4999999999929,82.5008729811058,-335.999999999996));
#32110=CARTESIAN_POINT('',(52.4999999999923,89.7177513459055,-338.5));
#32111=CARTESIAN_POINT('',(52.4999999999927,85.3876243270555,-338.499999999996));
#32112=CARTESIAN_POINT('',(52.499999999992,92.6045026919061,-333.5));
#32113=CARTESIAN_POINT('',(52.4999999999922,91.1611270189058,-336.));
#32114=CARTESIAN_POINT('',(52.4999999999923,89.7177513459067,-328.5));
#32115=CARTESIAN_POINT('',(52.4999999999922,91.1611270189064,-331.));
#32116=CARTESIAN_POINT('',(52.4999999999926,86.8310000000067,-328.499999999996));
#32117=CARTESIAN_POINT('Origin',(52.4999999999926,86.831000000001,-377.5));
#32118=CARTESIAN_POINT('',(52.4999999999928,83.9442486541016,-372.5));
#32119=CARTESIAN_POINT('',(52.4999999999931,81.057497308101,-377.5));
#32120=CARTESIAN_POINT('',(52.4999999999929,82.5008729811013,-375.));
#32121=CARTESIAN_POINT('',(52.4999999999928,83.9442486541005,-382.5));
#32122=CARTESIAN_POINT('',(52.4999999999929,82.5008729811008,-380.));
#32123=CARTESIAN_POINT('',(52.4999999999923,89.7177513459005,-382.5));
#32124=CARTESIAN_POINT('',(52.4999999999927,85.3876243270505,-382.5));
#32125=CARTESIAN_POINT('',(52.499999999992,92.604502691901,-377.5));
#32126=CARTESIAN_POINT('',(52.4999999999922,91.1611270189007,-380.));
#32127=CARTESIAN_POINT('',(52.4999999999923,89.7177513459016,-372.5));
#32128=CARTESIAN_POINT('',(52.4999999999922,91.1611270189013,-375.));
#32129=CARTESIAN_POINT('',(52.4999999999926,86.8310000000016,-372.5));
#32130=CARTESIAN_POINT('Origin',(43.9999999999906,109.330999999997,-404.964101615149));
#32131=CARTESIAN_POINT('',(45.9999999999906,109.330999999997,-406.118802153499));
#32132=CARTESIAN_POINT('',(41.9999999999906,109.330999999997,-403.809401076799));
#32133=CARTESIAN_POINT('',(45.9999999999906,109.330999999997,-406.118802153499));
#32134=CARTESIAN_POINT('',(41.9999999999906,109.330999999997,-403.809401076799));
#32135=CARTESIAN_POINT('',(45.9999999999906,109.330999999997,-406.118802153499));
#32136=CARTESIAN_POINT('Origin',(41.9999999999906,109.330999999997,-401.5));
#32137=CARTESIAN_POINT('',(41.9999999999906,109.330999999998,-399.190598923199));
#32138=CARTESIAN_POINT('',(41.9999999999906,109.330999999997,-402.957368983363));
#32139=CARTESIAN_POINT('',(41.9999999999906,109.330999999998,-399.190598923199));
#32140=CARTESIAN_POINT('Origin',(43.9999999999906,109.330999999998,-398.035898384849));
#32141=CARTESIAN_POINT('',(45.9999999999906,109.330999999998,-396.881197846499));
#32142=CARTESIAN_POINT('',(41.9999999999906,109.330999999998,-399.190598923199));
#32143=CARTESIAN_POINT('',(45.9999999999906,109.330999999998,-396.881197846499));
#32144=CARTESIAN_POINT('Origin',(47.9999999999906,109.330999999998,-398.035898384849));
#32145=CARTESIAN_POINT('',(49.9999999999906,109.330999999998,-399.190598923199));
#32146=CARTESIAN_POINT('',(45.9999999999906,109.330999999998,-396.881197846499));
#32147=CARTESIAN_POINT('',(49.9999999999906,109.330999999998,-399.190598923199));
#32148=CARTESIAN_POINT('Origin',(49.9999999999906,109.330999999998,-401.5));
#32149=CARTESIAN_POINT('',(49.9999999999906,109.330999999998,-403.809401076799));
#32150=CARTESIAN_POINT('',(49.9999999999906,109.330999999998,-402.957368983363));
#32151=CARTESIAN_POINT('',(49.9999999999906,109.330999999998,-403.809401076799));
#32152=CARTESIAN_POINT('Origin',(47.9999999999906,109.330999999997,-404.964101615149));
#32153=CARTESIAN_POINT('',(49.9999999999906,109.330999999998,-403.809401076799));
#32154=CARTESIAN_POINT('Origin',(50.4999999999899,117.331,-393.5));
#32155=CARTESIAN_POINT('',(54.9999999999906,109.331,-393.5));
#32156=CARTESIAN_POINT('',(54.9999999999905,110.331,-393.5));
#32157=CARTESIAN_POINT('',(54.9999999999899,117.331,-393.5));
#32158=CARTESIAN_POINT('',(44.9999999999906,109.330999999998,-393.5));
#32159=CARTESIAN_POINT('',(47.4573689833543,109.330999999999,-393.5));
#32160=CARTESIAN_POINT('',(44.9999999999899,117.330999999998,-393.5));
#32161=CARTESIAN_POINT('',(44.9999999999899,117.330999999998,-393.5));
#32162=CARTESIAN_POINT('',(47.9999999999899,117.330999999999,-393.5));
#32163=CARTESIAN_POINT('',(-1.50000000001011,117.330999999994,-393.5));
#32164=CARTESIAN_POINT('Origin',(47.9999999999905,110.330999999999,-393.5));
#32165=CARTESIAN_POINT('Origin',(44.9999999999899,117.330999999998,-400.5));
#32166=CARTESIAN_POINT('',(37.9999999999905,109.330999999997,-400.5));
#32167=CARTESIAN_POINT('',(37.9999999999899,117.330999999997,-400.5));
#32168=CARTESIAN_POINT('',(37.9999999999899,117.330999999997,-400.5));
#32169=CARTESIAN_POINT('Origin',(44.99999999999,117.330999999997,-400.5));
#32170=CARTESIAN_POINT('Origin',(44.9999999999907,109.330999999998,-400.499999999999));
#32171=CARTESIAN_POINT('Origin',(37.9999999999899,117.330999999996,-406.));
#32172=CARTESIAN_POINT('',(37.9999999999899,117.330999999997,-403.5));
#32173=CARTESIAN_POINT('',(37.9999999999899,117.331000000002,-355.5));
#32174=CARTESIAN_POINT('',(37.9999999999905,109.330999999996,-410.5));
#32175=CARTESIAN_POINT('',(37.9999999999905,109.330999999997,-402.957368983363));
#32176=CARTESIAN_POINT('',(37.9999999999905,110.330999999996,-410.5));
#32177=CARTESIAN_POINT('',(37.9999999999899,117.330999999996,-410.5));
#32178=CARTESIAN_POINT('Origin',(37.9999999999905,110.330999999997,-403.5));
#32179=CARTESIAN_POINT('Origin',(-47.0000000000094,109.330999999989,-404.964101615149));
#32180=CARTESIAN_POINT('',(-49.0000000000094,109.330999999989,-406.118802153499));
#32181=CARTESIAN_POINT('',(-45.0000000000094,109.330999999989,-403.809401076799));
#32182=CARTESIAN_POINT('',(-49.0000000000094,109.330999999989,-406.118802153499));
#32183=CARTESIAN_POINT('',(-49.0000000000094,109.330999999989,-406.118802153499));
#32184=CARTESIAN_POINT('',(-45.0000000000094,109.330999999989,-403.809401076799));
#32185=CARTESIAN_POINT('Origin',(-45.0000000000094,109.33099999999,-401.5));
#32186=CARTESIAN_POINT('',(-45.0000000000094,109.33099999999,-399.190598923199));
#32187=CARTESIAN_POINT('',(-45.0000000000094,109.330999999989,-402.957368983363));
#32188=CARTESIAN_POINT('',(-45.0000000000094,109.33099999999,-399.190598923199));
#32189=CARTESIAN_POINT('Origin',(-47.0000000000094,109.33099999999,-398.035898384849));
#32190=CARTESIAN_POINT('',(-49.0000000000094,109.33099999999,-396.881197846499));
#32191=CARTESIAN_POINT('',(-45.0000000000094,109.33099999999,-399.190598923199));
#32192=CARTESIAN_POINT('',(-49.0000000000094,109.33099999999,-396.881197846499));
#32193=CARTESIAN_POINT('Origin',(-51.0000000000094,109.33099999999,-398.035898384849));
#32194=CARTESIAN_POINT('',(-53.0000000000094,109.330999999989,-399.190598923199));
#32195=CARTESIAN_POINT('',(-49.0000000000094,109.33099999999,-396.881197846499));
#32196=CARTESIAN_POINT('',(-53.0000000000094,109.330999999989,-399.190598923199));
#32197=CARTESIAN_POINT('Origin',(-53.0000000000094,109.330999999989,-401.5));
#32198=CARTESIAN_POINT('',(-53.0000000000094,109.330999999989,-403.809401076799));
#32199=CARTESIAN_POINT('',(-53.0000000000094,109.330999999989,-402.957368983363));
#32200=CARTESIAN_POINT('',(-53.0000000000094,109.330999999989,-403.809401076799));
#32201=CARTESIAN_POINT('Origin',(-51.0000000000094,109.330999999989,-404.964101615149));
#32202=CARTESIAN_POINT('',(-53.0000000000094,109.330999999989,-403.809401076799));
#32203=CARTESIAN_POINT('Origin',(-53.5000000000094,109.33099999999,-393.5));
#32204=CARTESIAN_POINT('',(-48.0000000000101,117.33099999999,-393.5));
#32205=CARTESIAN_POINT('',(-51.0000000000101,117.33099999999,-393.5));
#32206=CARTESIAN_POINT('',(-1.50000000001011,117.330999999994,-393.5));
#32207=CARTESIAN_POINT('',(-48.0000000000094,109.33099999999,-393.5));
#32208=CARTESIAN_POINT('',(-48.0000000000094,109.33099999999,-393.5));
#32209=CARTESIAN_POINT('',(-58.0000000000094,109.330999999989,-393.5));
#32210=CARTESIAN_POINT('',(-50.4573689833731,109.33099999999,-393.5));
#32211=CARTESIAN_POINT('',(-58.0000000000095,110.330999999989,-393.5));
#32212=CARTESIAN_POINT('',(-58.0000000000094,109.330999999989,-393.5));
#32213=CARTESIAN_POINT('Origin',(-51.0000000000095,110.33099999999,-393.5));
#32214=CARTESIAN_POINT('Origin',(-48.0000000000094,109.33099999999,-400.5));
#32215=CARTESIAN_POINT('',(-41.0000000000101,117.33099999999,-400.5));
#32216=CARTESIAN_POINT('',(-41.0000000000094,109.33099999999,-400.5));
#32217=CARTESIAN_POINT('',(-41.0000000000094,109.33099999999,-400.5));
#32218=CARTESIAN_POINT('Origin',(-48.0000000000095,109.33099999999,-400.5));
#32219=CARTESIAN_POINT('Origin',(-48.0000000000101,117.33099999999,-400.500000000001));
#32220=CARTESIAN_POINT('Origin',(-41.0000000000094,109.33099999999,-406.));
#32221=CARTESIAN_POINT('',(-41.0000000000094,109.330999999989,-410.5));
#32222=CARTESIAN_POINT('',(-41.0000000000095,110.330999999989,-410.5));
#32223=CARTESIAN_POINT('',(-41.0000000000094,109.330999999989,-410.5));
#32224=CARTESIAN_POINT('',(-41.0000000000094,109.33099999999,-402.957368983363));
#32225=CARTESIAN_POINT('',(-41.0000000000101,117.33099999999,-403.5));
#32226=CARTESIAN_POINT('',(-41.0000000000101,117.330999999995,-355.5));
#32227=CARTESIAN_POINT('Origin',(-41.0000000000095,110.33099999999,-403.5));
#32228=CARTESIAN_POINT('Origin',(47.9999999999906,109.331000000008,-312.964101615149));
#32229=CARTESIAN_POINT('',(45.9999999999906,109.331000000008,-314.118802153499));
#32230=CARTESIAN_POINT('',(49.9999999999906,109.331000000008,-311.809401076799));
#32231=CARTESIAN_POINT('',(45.9999999999906,109.331000000008,-314.118802153499));
#32232=CARTESIAN_POINT('',(45.9999999999906,109.331000000008,-314.118802153499));
#32233=CARTESIAN_POINT('',(49.9999999999906,109.331000000008,-311.809401076799));
#32234=CARTESIAN_POINT('Origin',(49.9999999999906,109.331000000009,-309.5));
#32235=CARTESIAN_POINT('',(49.9999999999906,109.331000000009,-307.190598923199));
#32236=CARTESIAN_POINT('',(49.9999999999906,109.331000000009,-308.042631016635));
#32237=CARTESIAN_POINT('',(49.9999999999906,109.331000000009,-307.190598923199));
#32238=CARTESIAN_POINT('Origin',(47.9999999999906,109.331000000009,-306.035898384849));
#32239=CARTESIAN_POINT('',(45.9999999999906,109.331000000009,-304.881197846499));
#32240=CARTESIAN_POINT('',(49.9999999999906,109.331000000009,-307.190598923199));
#32241=CARTESIAN_POINT('',(45.9999999999906,109.331000000009,-304.881197846499));
#32242=CARTESIAN_POINT('Origin',(43.9999999999906,109.331000000008,-306.035898384849));
#32243=CARTESIAN_POINT('',(41.9999999999906,109.331000000008,-307.190598923199));
#32244=CARTESIAN_POINT('',(45.9999999999906,109.331000000009,-304.881197846499));
#32245=CARTESIAN_POINT('',(41.9999999999906,109.331000000008,-307.190598923199));
#32246=CARTESIAN_POINT('Origin',(41.9999999999906,109.331000000008,-309.5));
#32247=CARTESIAN_POINT('',(41.9999999999906,109.331000000008,-311.809401076799));
#32248=CARTESIAN_POINT('',(41.9999999999906,109.331000000008,-308.042631016635));
#32249=CARTESIAN_POINT('',(41.9999999999906,109.331000000008,-311.809401076799));
#32250=CARTESIAN_POINT('Origin',(43.9999999999906,109.331000000008,-312.964101615149));
#32251=CARTESIAN_POINT('',(41.9999999999906,109.331000000008,-311.809401076799));
#32252=CARTESIAN_POINT('Origin',(50.4999999999906,109.331000000008,-317.5));
#32253=CARTESIAN_POINT('',(44.9999999999899,117.331000000007,-317.5));
#32254=CARTESIAN_POINT('',(47.9999999999899,117.331000000007,-317.5));
#32255=CARTESIAN_POINT('',(-1.50000000001011,117.331000000003,-317.5));
#32256=CARTESIAN_POINT('',(44.9999999999906,109.331000000007,-317.5));
#32257=CARTESIAN_POINT('',(44.9999999999906,109.331000000007,-317.5));
#32258=CARTESIAN_POINT('',(54.9999999999906,109.331000000008,-317.5));
#32259=CARTESIAN_POINT('',(47.4573689833543,109.331000000007,-317.5));
#32260=CARTESIAN_POINT('',(54.9999999999905,110.331000000008,-317.5));
#32261=CARTESIAN_POINT('',(54.9999999999906,109.331000000008,-317.5));
#32262=CARTESIAN_POINT('Origin',(47.9999999999905,110.331000000007,-317.5));
#32263=CARTESIAN_POINT('Origin',(44.9999999999906,109.331000000008,-310.5));
#32264=CARTESIAN_POINT('',(37.9999999999899,117.331000000007,-310.5));
#32265=CARTESIAN_POINT('',(37.9999999999905,109.331000000007,-310.5));
#32266=CARTESIAN_POINT('',(37.9999999999905,109.331000000007,-310.5));
#32267=CARTESIAN_POINT('Origin',(44.9999999999906,109.331000000008,-310.5));
#32268=CARTESIAN_POINT('Origin',(44.9999999999899,117.331000000008,-310.500000000001));
#32269=CARTESIAN_POINT('Origin',(37.9999999999905,109.331000000008,-305.));
#32270=CARTESIAN_POINT('',(37.9999999999905,109.331000000009,-300.5));
#32271=CARTESIAN_POINT('',(37.9999999999905,110.331000000009,-300.5));
#32272=CARTESIAN_POINT('',(37.9999999999905,109.331000000009,-300.5));
#32273=CARTESIAN_POINT('',(37.9999999999905,109.331000000008,-308.042631016635));
#32274=CARTESIAN_POINT('',(37.9999999999899,117.331000000008,-307.5));
#32275=CARTESIAN_POINT('',(37.9999999999899,117.331000000002,-355.5));
#32276=CARTESIAN_POINT('Origin',(37.9999999999905,110.331000000008,-307.5));
#32277=CARTESIAN_POINT('Origin',(-1.50000000001011,117.330999999999,-355.5));
#32278=CARTESIAN_POINT('',(-58.0000000000101,117.330999999988,-403.5));
#32279=CARTESIAN_POINT('',(-51.0000000000101,117.331,-317.5));
#32280=CARTESIAN_POINT('',(-51.0000000000101,117.330999999988,-410.5));
#32281=CARTESIAN_POINT('',(-48.0000000000101,117.331,-317.5));
#32282=CARTESIAN_POINT('',(-53.5000000000101,117.330999999999,-317.5));
#32283=CARTESIAN_POINT('',(-41.0000000000101,117.331,-310.5));
#32284=CARTESIAN_POINT('Origin',(-48.0000000000101,117.331,-310.500000000001));
#32285=CARTESIAN_POINT('',(-41.0000000000101,117.331,-307.5));
#32286=CARTESIAN_POINT('',(-41.0000000000101,117.331000000001,-305.));
#32287=CARTESIAN_POINT('',(-58.0000000000101,117.331,-307.5));
#32288=CARTESIAN_POINT('',(47.9999999999899,117.331000000009,-300.5));
#32289=CARTESIAN_POINT('Origin',(-47.0000000000094,109.331,-312.964101615149));
#32290=CARTESIAN_POINT('',(-49.0000000000094,109.331,-314.118802153499));
#32291=CARTESIAN_POINT('',(-45.0000000000094,109.331,-311.809401076799));
#32292=CARTESIAN_POINT('',(-49.0000000000094,109.331,-314.118802153499));
#32293=CARTESIAN_POINT('',(-49.0000000000095,109.331,-314.118802153499));
#32294=CARTESIAN_POINT('',(-45.0000000000094,109.331,-311.809401076799));
#32295=CARTESIAN_POINT('Origin',(-45.0000000000094,109.331,-309.5));
#32296=CARTESIAN_POINT('',(-45.0000000000094,109.331,-307.190598923199));
#32297=CARTESIAN_POINT('',(-45.0000000000094,109.331,-308.042631016635));
#32298=CARTESIAN_POINT('',(-45.0000000000094,109.331,-307.190598923199));
#32299=CARTESIAN_POINT('Origin',(-47.0000000000094,109.331,-306.035898384849));
#32300=CARTESIAN_POINT('',(-49.0000000000094,109.331,-304.881197846499));
#32301=CARTESIAN_POINT('',(-45.0000000000094,109.331,-307.190598923199));
#32302=CARTESIAN_POINT('',(-49.0000000000094,109.331,-304.881197846499));
#32303=CARTESIAN_POINT('Origin',(-51.0000000000094,109.331,-306.035898384849));
#32304=CARTESIAN_POINT('',(-53.0000000000094,109.331,-307.190598923199));
#32305=CARTESIAN_POINT('',(-49.0000000000094,109.331,-304.881197846499));
#32306=CARTESIAN_POINT('',(-53.0000000000094,109.331,-307.190598923199));
#32307=CARTESIAN_POINT('Origin',(-53.0000000000094,109.331,-309.5));
#32308=CARTESIAN_POINT('',(-53.0000000000094,109.331,-311.809401076799));
#32309=CARTESIAN_POINT('',(-53.0000000000094,109.331,-308.042631016635));
#32310=CARTESIAN_POINT('',(-53.0000000000094,109.331,-311.809401076799));
#32311=CARTESIAN_POINT('Origin',(-51.0000000000094,109.331,-312.964101615149));
#32312=CARTESIAN_POINT('',(-53.0000000000094,109.331,-311.809401076799));
#32313=CARTESIAN_POINT('Origin',(-41.0000000000094,109.331000000001,-305.));
#32314=CARTESIAN_POINT('',(-41.0000000000094,109.331,-310.5));
#32315=CARTESIAN_POINT('',(-41.0000000000094,109.331,-310.5));
#32316=CARTESIAN_POINT('',(-41.0000000000094,109.331000000002,-300.5));
#32317=CARTESIAN_POINT('',(-41.0000000000094,109.331,-308.042631016635));
#32318=CARTESIAN_POINT('',(-41.0000000000095,110.331000000002,-300.5));
#32319=CARTESIAN_POINT('',(-41.0000000000094,109.331000000002,-300.5));
#32320=CARTESIAN_POINT('Origin',(-41.0000000000095,110.331000000001,-307.5));
#32321=CARTESIAN_POINT('Origin',(-48.0000000000094,109.331,-310.5));
#32322=CARTESIAN_POINT('',(-48.0000000000094,109.331,-317.5));
#32323=CARTESIAN_POINT('',(-48.0000000000094,109.331,-317.5));
#32324=CARTESIAN_POINT('Origin',(-48.0000000000094,109.331000000001,-310.5));
#32325=CARTESIAN_POINT('Origin',(-53.5000000000094,109.330999999999,-317.5));
#32326=CARTESIAN_POINT('',(-58.0000000000094,109.330999999998,-317.5));
#32327=CARTESIAN_POINT('',(-58.0000000000095,110.330999999998,-317.5));
#32328=CARTESIAN_POINT('',(-58.0000000000094,109.330999999998,-317.5));
#32329=CARTESIAN_POINT('',(-50.4573689833731,109.331,-317.5));
#32330=CARTESIAN_POINT('Origin',(-51.0000000000095,110.330999999999,-317.499999999999));
#32331=CARTESIAN_POINT('Origin',(26.6129405624652,-47.4885629631521,-461.499999999981));
#32332=CARTESIAN_POINT('',(29.2172650211785,-63.2751868616857,-462.49999999998));
#32333=CARTESIAN_POINT('',(29.2172650211786,-63.2751868616856,-461.49999999998));
#32334=CARTESIAN_POINT('',(37.9266490614509,-58.8022714621361,-462.49999999998));
#32335=CARTESIAN_POINT('',(37.9266490614509,-58.802271462136,-461.499999999981));
#32336=CARTESIAN_POINT('Origin',(26.6129405624651,-47.4885629631522,-462.499999999891));
#32337=CARTESIAN_POINT('Origin',(47.6332714621302,-49.0956490614551,-461.499999999982));
#32338=CARTESIAN_POINT('',(47.6332714621302,-49.0956490614552,-462.499999999982));
#32339=CARTESIAN_POINT('',(47.6332714621302,-49.0956490614551,-461.499999999981));
#32340=CARTESIAN_POINT('',(37.9266490614509,-58.8022714621361,-462.49999999998));
#32341=CARTESIAN_POINT('Origin',(36.3195629631445,-37.7819405624712,-461.499999999982));
#32342=CARTESIAN_POINT('',(52.1061868616782,-40.3862650211816,-462.499999999983));
#32343=CARTESIAN_POINT('',(52.1061868616778,-40.3862650211815,-461.499999999983));
#32344=CARTESIAN_POINT('Origin',(36.3195629631445,-37.7819405624713,-462.499999999905));
#32345=CARTESIAN_POINT('Origin',(-125.,-11.1690000000246,-461.499999999984));
#32346=CARTESIAN_POINT('',(52.1061868616731,18.0482650211651,-462.49999999999));
#32347=CARTESIAN_POINT('',(52.1061868616733,18.0482650211652,-461.499999999989));
#32348=CARTESIAN_POINT('Origin',(-125.000000000001,-11.1690000000256,-462.49999999969));
#32349=CARTESIAN_POINT('Origin',(36.3195629631399,15.4439405624519,-461.499999999988));
#32350=CARTESIAN_POINT('',(47.6332714621237,26.7576490614375,-462.49999999999));
#32351=CARTESIAN_POINT('',(47.6332714621237,26.7576490614377,-461.49999999999));
#32352=CARTESIAN_POINT('Origin',(36.3195629631398,15.4439405624517,-462.499999999907));
#32353=CARTESIAN_POINT('Origin',(37.9266490614429,36.4642714621169,-461.499999999991));
#32354=CARTESIAN_POINT('',(37.9266490614428,36.4642714621168,-462.499999999991));
#32355=CARTESIAN_POINT('',(37.9266490614428,36.4642714621169,-461.499999999991));
#32356=CARTESIAN_POINT('',(47.6332714621237,26.7576490614375,-462.49999999999));
#32357=CARTESIAN_POINT('Origin',(26.6129405624589,25.1505629631313,-461.499999999989));
#32358=CARTESIAN_POINT('',(29.2172650211694,40.9371868616652,-462.499999999991));
#32359=CARTESIAN_POINT('',(29.2172650211694,40.9371868616654,-461.499999999992));
#32360=CARTESIAN_POINT('Origin',(26.6129405624589,25.1505629631313,-462.499999999889));
#32361=CARTESIAN_POINT('Origin',(1.22402088464923E-11,-136.169000000013,
-461.499999999971));
#32362=CARTESIAN_POINT('',(-29.2172650211774,40.9371868616598,-462.499999999991));
#32363=CARTESIAN_POINT('',(-29.2172650211774,40.9371868616601,-461.499999999991));
#32364=CARTESIAN_POINT('Origin',(1.38211769938405E-11,-136.16900000002,
-462.499999998645));
#32365=CARTESIAN_POINT('Origin',(-26.6129405624642,25.1505629631266,-461.499999999989));
#32366=CARTESIAN_POINT('',(-37.9266490614499,36.4642714621103,-462.499999999991));
#32367=CARTESIAN_POINT('',(-37.9266490614499,36.4642714621104,-461.49999999999));
#32368=CARTESIAN_POINT('Origin',(-26.6129405624642,25.1505629631265,-462.499999999905));
#32369=CARTESIAN_POINT('Origin',(-47.6332714621292,26.7576490614295,-461.499999999989));
#32370=CARTESIAN_POINT('',(-47.6332714621292,26.7576490614294,-462.499999999989));
#32371=CARTESIAN_POINT('',(-47.6332714621292,26.7576490614296,-461.49999999999));
#32372=CARTESIAN_POINT('',(-37.9266490614499,36.4642714621103,-462.49999999999));
#32373=CARTESIAN_POINT('Origin',(-36.3195629631435,15.4439405624457,-461.499999999988));
#32374=CARTESIAN_POINT('Origin',(-36.3195629631436,15.4439405624456,-462.499999999891));
#32375=CARTESIAN_POINT('Origin',(-36.3195629631389,-37.7819405624774,-461.499999999982));
#32376=CARTESIAN_POINT('',(-47.6332714621227,-49.0956490614632,-462.49999999998));
#32377=CARTESIAN_POINT('',(-47.6332714621227,-49.0956490614631,-461.499999999981));
#32378=CARTESIAN_POINT('Origin',(-36.3195629631389,-37.7819405624776,-462.499999999884));
#32379=CARTESIAN_POINT('Origin',(-37.9266490614418,-58.8022714621425,-461.49999999998));
#32380=CARTESIAN_POINT('',(-37.9266490614418,-58.8022714621426,-462.49999999998));
#32381=CARTESIAN_POINT('',(-37.9266490614418,-58.8022714621425,-461.49999999998));
#32382=CARTESIAN_POINT('',(-47.6332714621227,-49.0956490614632,-462.49999999998));
#32383=CARTESIAN_POINT('Origin',(-26.612940562458,-47.4885629631568,-461.499999999981));
#32384=CARTESIAN_POINT('',(-29.2172650211685,-63.2751868616909,-462.499999999979));
#32385=CARTESIAN_POINT('',(-29.2172650211685,-63.2751868616907,-461.499999999979));
#32386=CARTESIAN_POINT('Origin',(-26.612940562458,-47.488562963157,-462.499999999894));
#32387=CARTESIAN_POINT('Origin',(-1.04360964314765E-11,113.830999999987,
-461.5));
#32388=CARTESIAN_POINT('Origin',(-1.14310418010589E-11,113.830999999992,
-462.499999998675));
#32389=CARTESIAN_POINT('Origin',(52.4999999999929,82.5008729811058,-335.999999999996));
#32390=CARTESIAN_POINT('',(55.1642481716112,83.9442486541057,-338.499999999996));
#32391=CARTESIAN_POINT('',(52.4999999999928,83.9442486541055,-338.499999999996));
#32392=CARTESIAN_POINT('',(55.1642481716032,81.0574973081063,-333.499999999996));
#32393=CARTESIAN_POINT('',(52.4999999999931,81.0574973081061,-333.499999999996));
#32394=CARTESIAN_POINT('Origin',(35.6399999999928,82.5008729811182,-336.00000000002));
#32395=CARTESIAN_POINT('Origin',(52.4999999999929,82.5008729811064,-330.999999999996));
#32396=CARTESIAN_POINT('',(55.1642481716112,83.9442486541069,-328.499999999996));
#32397=CARTESIAN_POINT('',(52.4999999999928,83.9442486541067,-328.499999999996));
#32398=CARTESIAN_POINT('Origin',(35.6399999999928,82.5008729811189,-330.999999999972));
#32399=CARTESIAN_POINT('Origin',(52.4999999999926,86.8310000000067,-328.499999999996));
#32400=CARTESIAN_POINT('',(55.1642481716107,89.7177513459069,-328.5));
#32401=CARTESIAN_POINT('',(52.4999999999923,89.7177513459067,-328.5));
#32402=CARTESIAN_POINT('Origin',(35.6399999998842,86.8310000000025,-328.500000000393));
#32403=CARTESIAN_POINT('Origin',(52.4999999999922,91.1611270189064,-331.));
#32404=CARTESIAN_POINT('',(55.1642481716022,92.6045026919063,-333.5));
#32405=CARTESIAN_POINT('',(52.499999999992,92.6045026919061,-333.5));
#32406=CARTESIAN_POINT('Origin',(35.639999999992,91.1611270188897,-330.999999999974));
#32407=CARTESIAN_POINT('Origin',(52.4999999999922,91.1611270189058,-336.));
#32408=CARTESIAN_POINT('',(55.1642481716107,89.7177513459057,-338.5));
#32409=CARTESIAN_POINT('',(52.4999999999923,89.7177513459055,-338.5));
#32410=CARTESIAN_POINT('Origin',(35.639999999992,91.1611270188918,-336.000000000022));
#32411=CARTESIAN_POINT('Origin',(52.4999999999927,85.3876243270555,-338.499999999996));
#32412=CARTESIAN_POINT('Origin',(35.6400000000029,86.8310000000037,-338.500000000075));
#32413=CARTESIAN_POINT('Origin',(52.4999999999929,82.5008729811008,-380.));
#32414=CARTESIAN_POINT('',(55.1642481716112,83.9442486541007,-382.5));
#32415=CARTESIAN_POINT('',(52.4999999999928,83.9442486541005,-382.5));
#32416=CARTESIAN_POINT('',(55.1642481716032,81.0574973081013,-377.5));
#32417=CARTESIAN_POINT('',(52.4999999999931,81.057497308101,-377.5));
#32418=CARTESIAN_POINT('Origin',(35.6399999999927,82.5008729811131,-380.000000000024));
#32419=CARTESIAN_POINT('Origin',(52.4999999999929,82.5008729811013,-375.));
#32420=CARTESIAN_POINT('',(55.1642481716112,83.9442486541018,-372.5));
#32421=CARTESIAN_POINT('',(52.4999999999928,83.9442486541016,-372.5));
#32422=CARTESIAN_POINT('Origin',(35.6399999999927,82.5008729811141,-374.999999999975));
#32423=CARTESIAN_POINT('Origin',(52.4999999999926,86.8310000000016,-372.5));
#32424=CARTESIAN_POINT('',(55.1642481716107,89.7177513459018,-372.5));
#32425=CARTESIAN_POINT('',(52.4999999999923,89.7177513459016,-372.5));
#32426=CARTESIAN_POINT('Origin',(35.6400000000052,86.8310000000011,-372.499999999934));
#32427=CARTESIAN_POINT('Origin',(52.4999999999922,91.1611270189013,-375.));
#32428=CARTESIAN_POINT('',(55.1642481716022,92.6045026919012,-377.5));
#32429=CARTESIAN_POINT('',(52.499999999992,92.604502691901,-377.5));
#32430=CARTESIAN_POINT('Origin',(35.639999999992,91.1611270188862,-374.999999999976));
#32431=CARTESIAN_POINT('Origin',(52.4999999999922,91.1611270189007,-380.));
#32432=CARTESIAN_POINT('',(55.1642481716107,89.7177513459007,-382.5));
#32433=CARTESIAN_POINT('',(52.4999999999923,89.7177513459005,-382.5));
#32434=CARTESIAN_POINT('Origin',(35.639999999992,91.1611270188853,-380.000000000024));
#32435=CARTESIAN_POINT('Origin',(52.4999999999927,85.3876243270505,-382.5));
#32436=CARTESIAN_POINT('Origin',(35.6400000000109,86.8309999999987,-382.500000000053));
#32437=CARTESIAN_POINT('Origin',(47.9999999999905,110.331000000009,-300.5));
#32438=CARTESIAN_POINT('',(54.9999999999905,110.331000000004,-355.5));
#32439=CARTESIAN_POINT('Origin',(-58.0000000000095,110.330999999988,-403.5));
#32440=CARTESIAN_POINT('',(-1.5000000000095,110.330999999992,-410.5));
#32441=CARTESIAN_POINT('Origin',(47.4573689833543,109.330999999998,-402.957368983363));
#32442=CARTESIAN_POINT('',(47.9999999999906,109.330999999997,-410.5));
#32443=CARTESIAN_POINT('',(54.9999999999906,109.330999999998,-403.5));
#32444=CARTESIAN_POINT('Origin',(47.9999999999906,109.330999999998,-403.500000000001));
#32445=CARTESIAN_POINT('',(-1.50000000000941,109.330999999992,-410.5));
#32446=CARTESIAN_POINT('',(54.9999999999906,109.331000000004,-355.5));
#32447=CARTESIAN_POINT('Origin',(-51.0000000000095,110.330999999988,-410.5));
#32448=CARTESIAN_POINT('',(-58.0000000000095,110.330999999994,-355.5));
#32449=CARTESIAN_POINT('Origin',(-50.4573689833731,109.330999999989,-402.957368983363));
#32450=CARTESIAN_POINT('',(-51.0000000000094,109.330999999988,-410.5));
#32451=CARTESIAN_POINT('',(-1.50000000000941,109.330999999992,-410.5));
#32452=CARTESIAN_POINT('',(-58.0000000000094,109.330999999988,-403.5));
#32453=CARTESIAN_POINT('Origin',(-51.0000000000094,109.330999999989,-403.500000000001));
#32454=CARTESIAN_POINT('',(-58.0000000000094,109.330999999994,-355.5));
#32455=CARTESIAN_POINT('Origin',(47.4573689833543,109.331000000009,-308.042631016635));
#32456=CARTESIAN_POINT('',(47.9999999999906,109.331000000009,-300.5));
#32457=CARTESIAN_POINT('',(-26.2500000000094,109.331000000003,-300.5));
#32458=CARTESIAN_POINT('',(54.9999999999906,109.331000000009,-307.5));
#32459=CARTESIAN_POINT('Origin',(47.9999999999906,109.331000000009,-307.500000000001));
#32460=CARTESIAN_POINT('',(54.9999999999906,109.331000000004,-355.5));
#32461=CARTESIAN_POINT('Origin',(-58.0000000000095,110.331,-307.5));
#32462=CARTESIAN_POINT('',(-26.2500000000095,110.331000000003,-300.5));
#32463=CARTESIAN_POINT('Origin',(-50.4573689833731,109.331,-308.042631016635));
#32464=CARTESIAN_POINT('',(-58.0000000000094,109.331,-307.5));
#32465=CARTESIAN_POINT('',(-58.0000000000094,109.330999999994,-355.5));
#32466=CARTESIAN_POINT('',(-51.0000000000094,109.331,-300.5));
#32467=CARTESIAN_POINT('Origin',(-51.0000000000095,109.331,-307.500000000001));
#32468=CARTESIAN_POINT('',(-26.2500000000094,109.331000000003,-300.5));
#32469=CARTESIAN_POINT('Origin',(-61.0064055375887,-63.6901241633721,-442.499999999978));
#32470=CARTESIAN_POINT('',(-53.0300791427081,-49.8747215894684,-462.499718596329));
#32471=CARTESIAN_POINT('',(-56.5529890060881,-55.976580463545,-455.455487085872));
#32472=CARTESIAN_POINT('Ctrl Pts',(-53.0302197456166,-49.8749651210668,
-462.499437315867));
#32473=CARTESIAN_POINT('Ctrl Pts',(-53.5772253220562,-50.8224065714837,
-461.405135361616));
#32474=CARTESIAN_POINT('Ctrl Pts',(-54.1391093421611,-51.7956182422464,
-460.281440602366));
#32475=CARTESIAN_POINT('Ctrl Pts',(-55.3014638055348,-53.8088752292143,
-457.95729552662));
#32476=CARTESIAN_POINT('Ctrl Pts',(-55.9378134738743,-54.9110651861781,
-456.685162782456));
#32477=CARTESIAN_POINT('Ctrl Pts',(-56.5529890060879,-55.9765804635453,
-455.455487085872));
#32478=CARTESIAN_POINT('',(-61.0064055375889,-63.6901241633744,-462.499999999978));
#32479=CARTESIAN_POINT('',(-61.0064055375889,-63.6901241633744,-462.499999999979));
#32480=CARTESIAN_POINT('',(-61.0064055375888,-63.6901241633726,-446.555000365155));
#32481=CARTESIAN_POINT('',(-61.0064055375887,-63.6901241633722,-442.499999999978));
#32482=CARTESIAN_POINT('Ctrl Pts',(-56.5529890060879,-55.9765804635452,
-455.455487085872));
#32483=CARTESIAN_POINT('Ctrl Pts',(-57.3037589083373,-57.2769520790348,
-453.954027830977));
#32484=CARTESIAN_POINT('Ctrl Pts',(-58.1291756986755,-58.7066158973974,
-452.303717577715));
#32485=CARTESIAN_POINT('Ctrl Pts',(-59.614164504551,-61.2786919578449,-449.335876617764));
#32486=CARTESIAN_POINT('Ctrl Pts',(-60.3130716773339,-62.4892346908032,
-447.93954461762));
#32487=CARTESIAN_POINT('Ctrl Pts',(-61.0064055375887,-63.6901241633725,
-446.555000365155));
#32488=CARTESIAN_POINT('Origin',(6.66133814775094E-13,-11.1690000000111,
-442.499999999986));
#32489=CARTESIAN_POINT('',(-52.5211241633496,-72.1754055376122,-462.499999999977));
#32490=CARTESIAN_POINT('Origin',(3.5527136788005E-13,-11.1690000000144,
-462.49999999999));
#32491=CARTESIAN_POINT('',(-52.5211241633495,-72.1754055376103,-446.554850154037));
#32492=CARTESIAN_POINT('',(-52.5211241633495,-72.1754055376099,-442.499999999978));
#32493=CARTESIAN_POINT('Ctrl Pts',(-61.0064055375888,-63.6901241633725,
-446.555000365155));
#32494=CARTESIAN_POINT('Ctrl Pts',(-59.7028303851691,-65.2043041369367,
-446.489771872832));
#32495=CARTESIAN_POINT('Ctrl Pts',(-58.3409919033042,-66.6719343927154,
-446.458142664235));
#32496=CARTESIAN_POINT('Ctrl Pts',(-55.5103141820403,-69.5031427304158,
-446.457920540329));
#32497=CARTESIAN_POINT('Ctrl Pts',(-54.0391111582702,-70.8685528762214,
-446.489484908003));
#32498=CARTESIAN_POINT('Ctrl Pts',(-52.5211241633495,-72.1754055376103,
-446.554850154037));
#32499=CARTESIAN_POINT('Origin',(-52.5211241633494,-72.1754055376099,-442.499999999978));
#32500=CARTESIAN_POINT('',(-38.7057432251289,-64.1990916340934,-462.499726017634));
#32501=CARTESIAN_POINT('',(-38.705506016167,-64.1989546813131,-462.499999999979));
#32502=CARTESIAN_POINT('',(-44.7374479018055,-67.6814979526866,-455.53635793138));
#32503=CARTESIAN_POINT('Ctrl Pts',(-44.7374479017809,-67.6814979527087,
-455.536357931381));
#32504=CARTESIAN_POINT('Ctrl Pts',(-43.6857872701621,-67.0743214039474,
-456.750069874714));
#32505=CARTESIAN_POINT('Ctrl Pts',(-42.5978914217962,-66.446224443087,-458.005729087235));
#32506=CARTESIAN_POINT('Ctrl Pts',(-40.6077271815802,-65.2972025832667,
-460.30325547882));
#32507=CARTESIAN_POINT('Ctrl Pts',(-39.6441515550798,-64.7408819358782,
-461.415842174298));
#32508=CARTESIAN_POINT('Ctrl Pts',(-38.7059803294307,-64.1992285262037,
-462.499452156896));
#32509=CARTESIAN_POINT('Ctrl Pts',(-52.5211241633495,-72.1754055376104,
-446.554850154037));
#32510=CARTESIAN_POINT('Ctrl Pts',(-51.309846368319,-71.4760739765861,-447.951355698663));
#32511=CARTESIAN_POINT('Ctrl Pts',(-50.0887918485801,-70.7710978208717,
-449.359814919897));
#32512=CARTESIAN_POINT('Ctrl Pts',(-47.4933387038742,-69.2726122491067,
-452.354661179647));
#32513=CARTESIAN_POINT('Ctrl Pts',(-46.0497544858338,-68.439158512271,-454.021075738748));
#32514=CARTESIAN_POINT('Ctrl Pts',(-44.7374479017856,-67.6814979527114,
-455.536357931375));
#32515=CARTESIAN_POINT('Origin',(52.5211241633613,-72.1754055376007,-442.49999999998));
#32516=CARTESIAN_POINT('',(52.5211241633611,-72.175405537603,-462.499999999979));
#32517=CARTESIAN_POINT('',(52.5211241633611,-72.175405537603,-462.499999999979));
#32518=CARTESIAN_POINT('',(52.5211241633613,-72.1754055376012,-446.555918723113));
#32519=CARTESIAN_POINT('',(52.5211241633614,-72.1754055376007,-442.499999999979));
#32520=CARTESIAN_POINT('Ctrl Pts',(44.737447901791,-67.6814979527004,-455.536357931383));
#32521=CARTESIAN_POINT('Ctrl Pts',(46.0484136650392,-68.4383843890099,-454.022827080102));
#32522=CARTESIAN_POINT('Ctrl Pts',(47.4933110155619,-69.2725962632375,-452.355109735904));
#32523=CARTESIAN_POINT('Ctrl Pts',(50.0889455884469,-70.7711865826099,-449.360409943347));
#32524=CARTESIAN_POINT('Ctrl Pts',(51.3099391726234,-71.4761275571605,-447.952177252778));
#32525=CARTESIAN_POINT('Ctrl Pts',(52.5211241633614,-72.1754055376012,-446.555918723113));
#32526=CARTESIAN_POINT('Origin',(6.66133814775094E-13,-11.1690000000111,
-442.499999999986));
#32527=CARTESIAN_POINT('',(61.006405537599,-63.6901241633638,-462.49999999998));
#32528=CARTESIAN_POINT('Origin',(-2.93098878501041E-13,-11.1690000000144,
-462.499999999992));
#32529=CARTESIAN_POINT('',(61.0064055375993,-63.6901241633619,-446.556015654869));
#32530=CARTESIAN_POINT('',(61.0064055375992,-63.6901241633614,-442.49999999998));
#32531=CARTESIAN_POINT('Ctrl Pts',(52.5211241633613,-72.1754055376012,-446.555918723113));
#32532=CARTESIAN_POINT('Ctrl Pts',(54.0377808744736,-70.8696981330166,-446.490122433087));
#32533=CARTESIAN_POINT('Ctrl Pts',(55.5077540668189,-69.5055188910036,-446.458279670062));
#32534=CARTESIAN_POINT('Ctrl Pts',(58.3386174884044,-66.6744930634029,-446.458344295615));
#32535=CARTESIAN_POINT('Ctrl Pts',(59.7017006172735,-65.2056164294591,-446.490203981457));
#32536=CARTESIAN_POINT('Ctrl Pts',(61.0064055375992,-63.6901241633618,-446.55601565487));
#32537=CARTESIAN_POINT('Origin',(61.0064055375992,-63.6901241633614,-442.49999999998));
#32538=CARTESIAN_POINT('Ctrl Pts',(61.0064055375992,-63.690124163362,-446.55601565487));
#32539=CARTESIAN_POINT('Ctrl Pts',(60.3129264164325,-62.4889830915135,-447.94070717192));
#32540=CARTESIAN_POINT('Ctrl Pts',(59.6139369007277,-61.2782977364298,-449.337050349079));
#32541=CARTESIAN_POINT('Ctrl Pts',(58.1287483302424,-58.7058756735295,-452.304951999478));
#32542=CARTESIAN_POINT('Ctrl Pts',(57.3027210262701,-57.2751544145364,-453.956286633532));
#32543=CARTESIAN_POINT('Ctrl Pts',(56.5529890060965,-55.9765804635349,-455.455487085874));
#32544=CARTESIAN_POINT('',(53.0295409752009,-49.8737894561974,-462.499999999981));
#32545=CARTESIAN_POINT('Origin',(61.0064055375901,41.3521241633499,-442.499999999992));
#32546=CARTESIAN_POINT('',(61.0064055375899,41.3521241633477,-462.499999999992));
#32547=CARTESIAN_POINT('',(61.0064055375899,41.3521241633477,-462.499999999992));
#32548=CARTESIAN_POINT('',(61.00640553759,41.3521241633499,-442.499999999992));
#32549=CARTESIAN_POINT('Origin',(6.66133814775094E-13,-11.1690000000111,
-442.499999999986));
#32550=CARTESIAN_POINT('',(52.5211241633506,49.8374055375854,-462.499999999993));
#32551=CARTESIAN_POINT('Origin',(2.91322521661641E-12,-11.1690000000106,
-462.49999999998));
#32552=CARTESIAN_POINT('',(52.5211241633507,49.8374055375877,-442.499999999993));
#32553=CARTESIAN_POINT('Origin',(52.5211241633508,49.8374055375877,-442.499999999993));
#32554=CARTESIAN_POINT('',(38.7052701169132,41.8608184847882,-462.499999999992));
#32555=CARTESIAN_POINT('Origin',(-52.5211241633601,49.8374055375786,-442.499999999991));
#32556=CARTESIAN_POINT('',(-43.5419127712896,44.6532698807934,-456.914899800777));
#32557=CARTESIAN_POINT('',(-38.7066184322078,41.8615969349749,-462.499999999991));
#32558=CARTESIAN_POINT('Ctrl Pts',(-43.5419565207299,44.6532806820063,-456.914942914046));
#32559=CARTESIAN_POINT('Ctrl Pts',(-43.3888210609314,44.5648678830691,-457.092282683389));
#32560=CARTESIAN_POINT('Ctrl Pts',(-43.260269592342,44.4906486580742,-457.241800248498));
#32561=CARTESIAN_POINT('Ctrl Pts',(-42.7372899671077,44.1887062306645,-457.847255790856));
#32562=CARTESIAN_POINT('Ctrl Pts',(-42.535915318321,44.0724425229795,-458.080116830013));
#32563=CARTESIAN_POINT('Ctrl Pts',(-41.9435098505755,43.7304170667072,-458.764642376408));
#32564=CARTESIAN_POINT('Ctrl Pts',(-41.4886182402114,43.4677852730115,-459.289573202535));
#32565=CARTESIAN_POINT('Ctrl Pts',(-40.3188335853071,42.7924097876085,-460.639149869349));
#32566=CARTESIAN_POINT('Ctrl Pts',(-39.5123048656016,42.3267602141773,-461.569029335436));
#32567=CARTESIAN_POINT('Ctrl Pts',(-38.7066184322079,41.861596934975,-462.499999999991));
#32568=CARTESIAN_POINT('',(-52.5211241633603,49.8374055375763,-462.499999999992));
#32569=CARTESIAN_POINT('',(-52.5211241633602,49.8374055375763,-462.499999999992));
#32570=CARTESIAN_POINT('',(-52.5211241633601,49.837405537578,-446.550390587012));
#32571=CARTESIAN_POINT('',(-52.5211241633601,49.8374055375786,-442.499999999991));
#32572=CARTESIAN_POINT('Ctrl Pts',(-43.5418850933958,44.6532394434158,-456.91486058488));
#32573=CARTESIAN_POINT('Ctrl Pts',(-45.0572774506985,45.5281516288324,-455.163894143534));
#32574=CARTESIAN_POINT('Ctrl Pts',(-46.7377899355917,46.4983959641712,-453.222925656717));
#32575=CARTESIAN_POINT('Ctrl Pts',(-49.7321482182746,48.2271895247285,-449.766679504493));
#32576=CARTESIAN_POINT('Ctrl Pts',(-51.1321942398983,49.0355064723819,-448.151530117407));
#32577=CARTESIAN_POINT('Ctrl Pts',(-52.5211241633599,49.837405537578,-446.550390587012));
#32578=CARTESIAN_POINT('Origin',(6.66133814775094E-13,-11.1690000000111,
-442.499999999986));
#32579=CARTESIAN_POINT('',(-61.0064055375982,41.352124163337,-462.499999999991));
#32580=CARTESIAN_POINT('Origin',(-2.38031816479634E-12,-11.1690000000101,
-462.499999999979));
#32581=CARTESIAN_POINT('',(-61.0064055375979,41.3521241633388,-446.553488658841));
#32582=CARTESIAN_POINT('',(-61.0064055375979,41.3521241633393,-442.49999999999));
#32583=CARTESIAN_POINT('Ctrl Pts',(-52.5211241633601,49.8374055375781,-446.550390587012));
#32584=CARTESIAN_POINT('Ctrl Pts',(-54.0643256331624,48.5088454414645,-446.486213866141));
#32585=CARTESIAN_POINT('Ctrl Pts',(-55.5591057416034,47.1198261279319,-446.455982678674));
#32586=CARTESIAN_POINT('Ctrl Pts',(-58.3862727598194,44.2851113555294,-446.459187956062));
#32587=CARTESIAN_POINT('Ctrl Pts',(-59.7244711699984,42.8411670798447,-446.490453383587));
#32588=CARTESIAN_POINT('Ctrl Pts',(-61.006405537598,41.3521241633388,-446.553488658841));
#32589=CARTESIAN_POINT('Origin',(-61.0064055375979,41.3521241633393,-442.49999999999));
#32590=CARTESIAN_POINT('',(-56.5529890060949,33.6385804635094,-455.455487085884));
#32591=CARTESIAN_POINT('Ctrl Pts',(-61.0064055375978,41.3521241633387,-446.553488658841));
#32592=CARTESIAN_POINT('Ctrl Pts',(-60.3110035926517,40.1476526630098,-447.942369697286));
#32593=CARTESIAN_POINT('Ctrl Pts',(-59.6106476791202,38.9346006374547,-449.341816313449));
#32594=CARTESIAN_POINT('Ctrl Pts',(-58.1300841047959,36.3701893028892,-452.30131448445));
#32595=CARTESIAN_POINT('Ctrl Pts',(-57.3381109788292,34.9984516104232,-453.885022424417));
#32596=CARTESIAN_POINT('Ctrl Pts',(-56.5529890060949,33.6385804635089,-455.455487085883));
#32597=CARTESIAN_POINT('',(-53.0305574330481,27.5375500128072,-462.499999999989));
#32598=CARTESIAN_POINT('',(-53.030557433048,27.537550012807,-462.499999999989));
#32599=CARTESIAN_POINT('Ctrl Pts',(-56.5529890060952,33.6385804635093,-455.455487085884));
#32600=CARTESIAN_POINT('Ctrl Pts',(-55.9412708023145,32.5790534546464,-456.678496830178));
#32601=CARTESIAN_POINT('Ctrl Pts',(-55.3067518807507,31.4800344443309,-457.947209569429));
#32602=CARTESIAN_POINT('Ctrl Pts',(-54.1447199575835,29.4673361133885,-460.271113052516));
#32603=CARTESIAN_POINT('Ctrl Pts',(-53.5798271593038,28.4889130857417,-461.401007474302));
#32604=CARTESIAN_POINT('Ctrl Pts',(-53.0305574330482,27.5375500128075,-462.499999999989));
#32605=CARTESIAN_POINT('Origin',(-104.132690000718,86.3051835969643,-462.5));
#32606=CARTESIAN_POINT('',(12.0150531445647,47.9060664143426,-462.499999999992));
#32607=CARTESIAN_POINT('',(18.8780323271008,47.6380911509506,-462.499968784806));
#32608=CARTESIAN_POINT('Ctrl Pts',(12.0150531445629,47.906066414339,-462.499999999997));
#32609=CARTESIAN_POINT('Ctrl Pts',(12.3401897703731,47.7470231052897,-462.499999999997));
#32610=CARTESIAN_POINT('Ctrl Pts',(13.4663873030089,47.1961341237507,-462.499999999997));
#32611=CARTESIAN_POINT('Ctrl Pts',(15.7097574528983,47.0181411184891,-462.499999999997));
#32612=CARTESIAN_POINT('Ctrl Pts',(16.3411029419287,47.0389120836614,-462.499999999997));
#32613=CARTESIAN_POINT('Ctrl Pts',(17.8946098878202,47.2634700470991,-462.499999999997));
#32614=CARTESIAN_POINT('Ctrl Pts',(18.3628654099176,47.4345106517495,-462.499999999997));
#32615=CARTESIAN_POINT('Ctrl Pts',(18.8780355053135,47.6380912035477,-462.499999999997));
#32616=CARTESIAN_POINT('Ctrl Pts',(31.7952304123374,45.4237242247432,-462.499999999997));
#32617=CARTESIAN_POINT('Ctrl Pts',(25.3169775513725,46.8233621997,-462.499999999997));
#32618=CARTESIAN_POINT('Ctrl Pts',(18.8780323213069,47.6380669487686,-462.499999999997));
#32619=CARTESIAN_POINT('Ctrl Pts',(56.5915605594614,20.625879662293,-462.499999999994));
#32620=CARTESIAN_POINT('Ctrl Pts',(56.3136127711561,21.9073690239263,-462.499999999994));
#32621=CARTESIAN_POINT('Ctrl Pts',(55.8688443804651,23.1467900735692,-462.500000000367));
#32622=CARTESIAN_POINT('Ctrl Pts',(54.6666325419165,25.4805815867024,-462.500000000368));
#32623=CARTESIAN_POINT('Ctrl Pts',(53.9138954951052,26.5642794410027,-462.499999999995));
#32624=CARTESIAN_POINT('Ctrl Pts',(53.0293871551266,27.5359584349847,-462.499999999995));
#32625=CARTESIAN_POINT('',(57.7295804999065,14.830443173281,-462.499999999989));
#32626=CARTESIAN_POINT('Origin',(-90.0000000001335,-11.1690000000447,-462.499999999809));
#32627=CARTESIAN_POINT('',(58.3152526334991,7.11256737781201,-462.499999999988));
#32628=CARTESIAN_POINT('Ctrl Pts',(57.7295804999045,14.8304431732815,-462.499999999993));
#32629=CARTESIAN_POINT('Ctrl Pts',(57.4005325308538,13.5557935149812,-462.499999999993));
#32630=CARTESIAN_POINT('Ctrl Pts',(57.283465559692,12.2356510331148,-462.499999999992));
#32631=CARTESIAN_POINT('Ctrl Pts',(57.4826884205102,9.61033012876741,-462.499999999992));
#32632=CARTESIAN_POINT('Ctrl Pts',(57.7976276531099,8.32296394996483,-462.499999999993));
#32633=CARTESIAN_POINT('Ctrl Pts',(58.3152526334968,7.11256737781103,-462.499999999993));
#32634=CARTESIAN_POINT('',(59.0902650976006,-0.703506953302192,-462.499999999987));
#32635=CARTESIAN_POINT('Ctrl Pts',(58.3152526334968,7.11256737781104,-462.499999999993));
#32636=CARTESIAN_POINT('Ctrl Pts',(58.8390772674901,5.88767374744325,-462.499999999992));
#32637=CARTESIAN_POINT('Ctrl Pts',(59.1725049660372,4.58984165948011,-462.499999999988));
#32638=CARTESIAN_POINT('Ctrl Pts',(59.435407607139,1.93844399318233,-462.499999999988));
#32639=CARTESIAN_POINT('Ctrl Pts',(59.3633429804589,0.600404665165133,-462.499999999992));
#32640=CARTESIAN_POINT('Ctrl Pts',(59.0902650975989,-0.703506953301665,
-462.499999999992));
#32641=CARTESIAN_POINT('',(59.406405003267,-7.27543664706474,-462.499999999987));
#32642=CARTESIAN_POINT('Ctrl Pts',(59.0902650975988,-0.703506953301827,
-462.499999999992));
#32643=CARTESIAN_POINT('Ctrl Pts',(58.8627320990774,-1.78994763186904,-462.499999999992));
#32644=CARTESIAN_POINT('Ctrl Pts',(58.7745669265647,-2.90096756015087,-462.499999999988));
#32645=CARTESIAN_POINT('Ctrl Pts',(58.8812368083505,-5.11842556204558,-462.499999999987));
#32646=CARTESIAN_POINT('Ctrl Pts',(59.0756383970967,-6.21585273547284,-462.499999999991));
#32647=CARTESIAN_POINT('Ctrl Pts',(59.4064050032652,-7.27543664706531,-462.499999999991));
#32648=CARTESIAN_POINT('',(59.4064050032676,-15.0625633529524,-462.499999999986));
#32649=CARTESIAN_POINT('Ctrl Pts',(59.4064050032652,-7.27543664706531,-462.499999999991));
#32650=CARTESIAN_POINT('Ctrl Pts',(59.7998586504781,-8.53583339440735,-462.499999999991));
#32651=CARTESIAN_POINT('Ctrl Pts',(60.0000000000047,-9.84861909545626,-462.499999999987));
#32652=CARTESIAN_POINT('Ctrl Pts',(59.9999999999965,-12.4893809046158,-462.499999999986));
#32653=CARTESIAN_POINT('Ctrl Pts',(59.7998586504701,-13.8021666056362,-462.49999999999));
#32654=CARTESIAN_POINT('Ctrl Pts',(59.4064050032657,-15.0625633529518,-462.49999999999));
#32655=CARTESIAN_POINT('',(59.0902650976022,-21.6344930467149,-462.499999999985));
#32656=CARTESIAN_POINT('Ctrl Pts',(59.4064050032657,-15.0625633529518,-462.49999999999));
#32657=CARTESIAN_POINT('Ctrl Pts',(59.0756383970974,-16.1221472645443,-462.49999999999));
#32658=CARTESIAN_POINT('Ctrl Pts',(58.8812368083515,-17.2195744379716,-462.499999999986));
#32659=CARTESIAN_POINT('Ctrl Pts',(58.7745669265659,-19.4370324398664,-462.499999999985));
#32660=CARTESIAN_POINT('Ctrl Pts',(58.8627320990786,-20.5480523681482,-462.499999999989));
#32661=CARTESIAN_POINT('Ctrl Pts',(59.0902650976002,-21.6344930467154,-462.499999999989));
#32662=CARTESIAN_POINT('Ctrl Pts',(59.0902650976002,-21.6344930467154,-462.499999999989));
#32663=CARTESIAN_POINT('Ctrl Pts',(59.3633429804669,-22.9384046652121,-462.499999999989));
#32664=CARTESIAN_POINT('Ctrl Pts',(59.4354076071443,-24.2764439932607,-462.499999999985));
#32665=CARTESIAN_POINT('Ctrl Pts',(59.1725049660245,-26.9278416595568,-462.499999999984));
#32666=CARTESIAN_POINT('Ctrl Pts',(58.8390772674808,-28.2256737474886,-462.499999999989));
#32667=CARTESIAN_POINT('Ctrl Pts',(58.3152526334998,-29.4505673778284,-462.499999999988));
#32668=CARTESIAN_POINT('Origin',(-89.9999999999107,-11.1690000000371,-462.499999999983));
#32669=CARTESIAN_POINT('Ctrl Pts',(53.0293871551332,-49.8739584350024,-462.499999999986));
#32670=CARTESIAN_POINT('Ctrl Pts',(53.9138954951112,-48.9022794410202,-462.499999999986));
#32671=CARTESIAN_POINT('Ctrl Pts',(54.6666325419227,-47.8185815867197,-462.500000000359));
#32672=CARTESIAN_POINT('Ctrl Pts',(55.8688443804717,-45.4847900735855,-462.50000000036));
#32673=CARTESIAN_POINT('Ctrl Pts',(56.3136127711626,-44.2453690239416,-462.499999999987));
#32674=CARTESIAN_POINT('Ctrl Pts',(56.5915605594671,-42.9638796623099,-462.499999999987));
#32675=CARTESIAN_POINT('Ctrl Pts',(31.7948796623067,-67.7605605594739,-462.499999999984));
#32676=CARTESIAN_POINT('Ctrl Pts',(33.0765842486482,-67.4825660901477,-462.499999999984));
#32677=CARTESIAN_POINT('Ctrl Pts',(34.3163262618311,-67.0376689797928,-462.500000000349));
#32678=CARTESIAN_POINT('Ctrl Pts',(36.650042374503,-65.8354478699916,-462.500000000349));
#32679=CARTESIAN_POINT('Ctrl Pts',(37.7336254438657,-65.082830891689,-462.499999999984));
#32680=CARTESIAN_POINT('Ctrl Pts',(38.7049734414089,-64.1983982826292,-462.499999999984));
#32681=CARTESIAN_POINT('',(25.9994431732944,-68.8985804999195,-462.499999999979));
#32682=CARTESIAN_POINT('Origin',(-5.05551156493311E-11,78.8310000002275,
-462.500000000346));
#32683=CARTESIAN_POINT('',(18.2815673778257,-69.4842526335121,-462.499999999979));
#32684=CARTESIAN_POINT('Ctrl Pts',(25.999443173295,-68.8985804999172,-462.499999999984));
#32685=CARTESIAN_POINT('Ctrl Pts',(24.7247935149947,-68.5695325308664,-462.499999999984));
#32686=CARTESIAN_POINT('Ctrl Pts',(23.4046510331284,-68.4524655597047,-462.499999999982));
#32687=CARTESIAN_POINT('Ctrl Pts',(20.779330128781,-68.6516884205231,-462.499999999982));
#32688=CARTESIAN_POINT('Ctrl Pts',(19.4919639499785,-68.9666276531229,-462.499999999983));
#32689=CARTESIAN_POINT('Ctrl Pts',(18.2815673778248,-69.4842526335099,-462.499999999983));
#32690=CARTESIAN_POINT('',(10.4654930467115,-70.2592650976135,-462.499999999979));
#32691=CARTESIAN_POINT('Ctrl Pts',(18.2815673778248,-69.4842526335099,-462.499999999983));
#32692=CARTESIAN_POINT('Ctrl Pts',(17.056673747458,-70.0080772675025,-462.499999999983));
#32693=CARTESIAN_POINT('Ctrl Pts',(15.7588416594962,-70.3415049660496,-462.499999999978));
#32694=CARTESIAN_POINT('Ctrl Pts',(13.1074439931985,-70.604407607152,-462.499999999978));
#32695=CARTESIAN_POINT('Ctrl Pts',(11.7694046651801,-70.5323429804717,-462.499999999983));
#32696=CARTESIAN_POINT('Ctrl Pts',(10.4654930467121,-70.2592650976111,-462.499999999983));
#32697=CARTESIAN_POINT('',(3.89356335294888,-70.5754050032799,-462.499999999978));
#32698=CARTESIAN_POINT('Ctrl Pts',(10.465493046712,-70.2592650976111,-462.499999999983));
#32699=CARTESIAN_POINT('Ctrl Pts',(9.37905236814473,-70.0317320990898,-462.499999999983));
#32700=CARTESIAN_POINT('Ctrl Pts',(8.26803243986281,-69.9435669265776,-462.499999999978));
#32701=CARTESIAN_POINT('Ctrl Pts',(6.05057443796808,-70.0502368083634,-462.499999999978));
#32702=CARTESIAN_POINT('Ctrl Pts',(4.95314726454063,-70.2446383971091,-462.499999999983));
#32703=CARTESIAN_POINT('Ctrl Pts',(3.89356335294815,-70.5754050032776,-462.499999999983));
#32704=CARTESIAN_POINT('',(-3.89356335293881,-70.5754050032805,-462.499999999978));
#32705=CARTESIAN_POINT('Ctrl Pts',(3.89356335294815,-70.5754050032776,-462.499999999983));
#32706=CARTESIAN_POINT('Ctrl Pts',(2.63316660560615,-70.9688586504905,-462.499999999983));
#32707=CARTESIAN_POINT('Ctrl Pts',(1.32038090455743,-71.1690000000175,-462.499999999978));
#32708=CARTESIAN_POINT('Ctrl Pts',(-1.32038090460214,-71.1690000000094,
-462.499999999978));
#32709=CARTESIAN_POINT('Ctrl Pts',(-2.63316660562244,-70.9688586504828,
-462.499999999983));
#32710=CARTESIAN_POINT('Ctrl Pts',(-3.89356335293808,-70.5754050032782,
-462.499999999983));
#32711=CARTESIAN_POINT('',(-10.4654930467012,-70.2592650976151,-462.499999999978));
#32712=CARTESIAN_POINT('Ctrl Pts',(-3.89356335293809,-70.5754050032782,
-462.499999999983));
#32713=CARTESIAN_POINT('Ctrl Pts',(-4.9531472645306,-70.24463839711,-462.499999999983));
#32714=CARTESIAN_POINT('Ctrl Pts',(-6.05057443795802,-70.0502368083644,
-462.499999999979));
#32715=CARTESIAN_POINT('Ctrl Pts',(-8.26803243985268,-69.9435669265789,
-462.499999999979));
#32716=CARTESIAN_POINT('Ctrl Pts',(-9.37905236813454,-70.0317320990914,
-462.499999999983));
#32717=CARTESIAN_POINT('Ctrl Pts',(-10.4654930467017,-70.2592650976128,
-462.499999999983));
#32718=CARTESIAN_POINT('',(-18.2815673778157,-69.4842526335148,-462.499999999978));
#32719=CARTESIAN_POINT('Ctrl Pts',(-10.4654930467017,-70.2592650976128,
-462.499999999983));
#32720=CARTESIAN_POINT('Ctrl Pts',(-11.7694046651997,-70.5323429804799,
-462.499999999983));
#32721=CARTESIAN_POINT('Ctrl Pts',(-13.1074439932496,-70.6044076071573,
-462.499999999978));
#32722=CARTESIAN_POINT('Ctrl Pts',(-15.7588416595456,-70.3415049660368,
-462.499999999978));
#32723=CARTESIAN_POINT('Ctrl Pts',(-17.0566737474761,-70.0080772674932,
-462.499999999983));
#32724=CARTESIAN_POINT('Ctrl Pts',(-18.2815673778148,-69.4842526335129,
-462.499999999983));
#32725=CARTESIAN_POINT('',(-25.9994431732854,-68.8985804999237,-462.499999999979));
#32726=CARTESIAN_POINT('Ctrl Pts',(-18.2815673778149,-69.4842526335129,
-462.499999999983));
#32727=CARTESIAN_POINT('Ctrl Pts',(-19.4919639499688,-68.966627653126,-462.499999999983));
#32728=CARTESIAN_POINT('Ctrl Pts',(-20.7793301287716,-68.6516884205264,
-462.499999999982));
#32729=CARTESIAN_POINT('Ctrl Pts',(-23.4046510331192,-68.4524655597085,
-462.499999999982));
#32730=CARTESIAN_POINT('Ctrl Pts',(-24.7247935149856,-68.5695325308705,
-462.499999999983));
#32731=CARTESIAN_POINT('Ctrl Pts',(-25.9994431732859,-68.8985804999215,
-462.499999999983));
#32732=CARTESIAN_POINT('',(-31.7948796622966,-67.7605605594826,-462.499999999979));
#32733=CARTESIAN_POINT('Origin',(-1.99706917669573E-11,78.8309999999131,
-462.500000001079));
#32734=CARTESIAN_POINT('Ctrl Pts',(-38.7057432251289,-64.1990916340934,
-462.499726017634));
#32735=CARTESIAN_POINT('Ctrl Pts',(-36.7423174004781,-65.9851579023194,
-462.499999999979));
#32736=CARTESIAN_POINT('Ctrl Pts',(-34.3848293251332,-67.1988151387573,
-462.499999999979));
#32737=CARTESIAN_POINT('Ctrl Pts',(-31.7948796622966,-67.7605605594826,
-462.499999999979));
#32738=CARTESIAN_POINT('',(-56.5915605594633,-42.9638796623205,-462.499999999981));
#32739=CARTESIAN_POINT('Ctrl Pts',(-56.5915605594633,-42.9638796623205,
-462.499999999981));
#32740=CARTESIAN_POINT('Ctrl Pts',(-56.029715455103,-45.5542889205284,-462.49999999998));
#32741=CARTESIAN_POINT('Ctrl Pts',(-54.8157369429699,-47.9121350536181,
-462.49999999998));
#32742=CARTESIAN_POINT('Ctrl Pts',(-53.0300791427081,-49.8747215894684,
-462.499718596329));
#32743=CARTESIAN_POINT('',(-57.7295804999055,-37.1684431733084,-462.499999999981));
#32744=CARTESIAN_POINT('Origin',(90.0000000000961,-11.1689999999847,-462.499999999614));
#32745=CARTESIAN_POINT('',(-58.315252633498,-29.4505673778391,-462.499999999982));
#32746=CARTESIAN_POINT('Ctrl Pts',(-57.7295804999029,-37.1684431733091,
-462.499999999986));
#32747=CARTESIAN_POINT('Ctrl Pts',(-57.4005325308522,-35.8937935150087,
-462.499999999986));
#32748=CARTESIAN_POINT('Ctrl Pts',(-57.2834655596905,-34.5736510331422,
-462.499999999985));
#32749=CARTESIAN_POINT('Ctrl Pts',(-57.4826884205089,-31.9483301287947,
-462.499999999986));
#32750=CARTESIAN_POINT('Ctrl Pts',(-57.7976276531085,-30.6609639499919,
-462.499999999987));
#32751=CARTESIAN_POINT('Ctrl Pts',(-58.3152526334954,-29.4505673778381,
-462.499999999987));
#32752=CARTESIAN_POINT('',(-59.0902650975996,-21.6344930467249,-462.499999999983));
#32753=CARTESIAN_POINT('Ctrl Pts',(-58.3152526334954,-29.4505673778381,
-462.499999999987));
#32754=CARTESIAN_POINT('Ctrl Pts',(-58.8390772674878,-28.2256737474723,
-462.499999999987));
#32755=CARTESIAN_POINT('Ctrl Pts',(-59.1725049660351,-26.9278416595116,
-462.499999999982));
#32756=CARTESIAN_POINT('Ctrl Pts',(-59.4354076071382,-24.2764439932139,
-462.499999999982));
#32757=CARTESIAN_POINT('Ctrl Pts',(-59.3633429804578,-22.9384046651945,
-462.499999999988));
#32758=CARTESIAN_POINT('Ctrl Pts',(-59.0902650975972,-21.6344930467255,
-462.499999999988));
#32759=CARTESIAN_POINT('',(-59.4064050032661,-15.0625633529624,-462.499999999984));
#32760=CARTESIAN_POINT('Ctrl Pts',(-59.0902650975972,-21.6344930467254,
-462.499999999988));
#32761=CARTESIAN_POINT('Ctrl Pts',(-58.8627320990759,-20.5480523681582,
-462.499999999988));
#32762=CARTESIAN_POINT('Ctrl Pts',(-58.7745669265638,-19.4370324398763,
-462.499999999983));
#32763=CARTESIAN_POINT('Ctrl Pts',(-58.8812368083496,-17.2195744379816,
-462.499999999984));
#32764=CARTESIAN_POINT('Ctrl Pts',(-59.0756383970952,-16.1221472645542,
-462.499999999989));
#32765=CARTESIAN_POINT('Ctrl Pts',(-59.4064050032639,-15.0625633529618,
-462.499999999989));
#32766=CARTESIAN_POINT('',(-59.4064050032667,-7.27543664707476,-462.499999999985));
#32767=CARTESIAN_POINT('Ctrl Pts',(-59.4064050032639,-15.0625633529618,
-462.499999999989));
#32768=CARTESIAN_POINT('Ctrl Pts',(-59.7998586504767,-13.8021666056197,
-462.499999999989));
#32769=CARTESIAN_POINT('Ctrl Pts',(-60.0000000000037,-12.489380904571,-462.499999999984));
#32770=CARTESIAN_POINT('Ctrl Pts',(-59.9999999999956,-9.84861909541142,
-462.499999999985));
#32771=CARTESIAN_POINT('Ctrl Pts',(-59.7998586504689,-8.53583339439112,
-462.49999999999));
#32772=CARTESIAN_POINT('Ctrl Pts',(-59.4064050032645,-7.27543664707546,
-462.49999999999));
#32773=CARTESIAN_POINT('',(-59.0902650976014,-0.703506953312267,-462.499999999986));
#32774=CARTESIAN_POINT('Ctrl Pts',(-59.4064050032645,-7.27543664707543,
-462.49999999999));
#32775=CARTESIAN_POINT('Ctrl Pts',(-59.0756383970961,-6.21585273548295,
-462.49999999999));
#32776=CARTESIAN_POINT('Ctrl Pts',(-58.8812368083507,-5.11842556205552,
-462.499999999985));
#32777=CARTESIAN_POINT('Ctrl Pts',(-58.7745669265651,-2.90096756016081,
-462.499999999985));
#32778=CARTESIAN_POINT('Ctrl Pts',(-58.8627320990773,-1.7899476318789,-462.49999999999));
#32779=CARTESIAN_POINT('Ctrl Pts',(-59.0902650975988,-0.703506953311725,
-462.49999999999));
#32780=CARTESIAN_POINT('',(-58.3152526335012,7.11256737780218,-462.499999999987));
#32781=CARTESIAN_POINT('Ctrl Pts',(-59.0902650975988,-0.703506953311577,
-462.49999999999));
#32782=CARTESIAN_POINT('Ctrl Pts',(-59.3633429804661,0.600404665187346,
-462.499999999991));
#32783=CARTESIAN_POINT('Ctrl Pts',(-59.4354076071438,1.93844399323813,-462.499999999986));
#32784=CARTESIAN_POINT('Ctrl Pts',(-59.1725049660226,4.58984165953402,-462.499999999986));
#32785=CARTESIAN_POINT('Ctrl Pts',(-58.8390772674787,5.88767374746334,-462.499999999991));
#32786=CARTESIAN_POINT('Ctrl Pts',(-58.3152526334986,7.11256737780097,-462.499999999991));
#32787=CARTESIAN_POINT('',(-57.7295804999101,14.8304431732717,-462.499999999987));
#32788=CARTESIAN_POINT('Ctrl Pts',(-58.3152526334985,7.11256737780111,-462.499999999991));
#32789=CARTESIAN_POINT('Ctrl Pts',(-57.7976276531118,8.32296394995511,-462.499999999991));
#32790=CARTESIAN_POINT('Ctrl Pts',(-57.4826884205125,9.61033012875785,-462.499999999991));
#32791=CARTESIAN_POINT('Ctrl Pts',(-57.2834655596947,12.2356510331055,-462.499999999991));
#32792=CARTESIAN_POINT('Ctrl Pts',(-57.4005325308566,13.555793514972,-462.499999999992));
#32793=CARTESIAN_POINT('Ctrl Pts',(-57.7295804999076,14.8304431732723,-462.499999999992));
#32794=CARTESIAN_POINT('',(-56.5915605594688,20.6258796622837,-462.499999999988));
#32795=CARTESIAN_POINT('Origin',(90.0000000001139,-11.1690000000374,-462.499999998157));
#32796=CARTESIAN_POINT('Ctrl Pts',(-53.0305574330451,27.5375500128045,-462.499999999994));
#32797=CARTESIAN_POINT('Ctrl Pts',(-53.9136598402457,26.5661625983044,-462.499999999994));
#32798=CARTESIAN_POINT('Ctrl Pts',(-54.6654949545811,25.4831869345778,-462.500000000018));
#32799=CARTESIAN_POINT('Ctrl Pts',(-55.867938981057,23.1493254197733,-462.500000000018));
#32800=CARTESIAN_POINT('Ctrl Pts',(-56.3133319485292,21.9086637678552,-462.499999999993));
#32801=CARTESIAN_POINT('Ctrl Pts',(-56.5915605594654,20.625879662283,-462.499999999993));
#32802=CARTESIAN_POINT('',(-31.7948796623065,45.4225605594505,-462.499999999992));
#32803=CARTESIAN_POINT('Ctrl Pts',(-38.7066184322078,41.8615969349749,-462.499999999991));
#32804=CARTESIAN_POINT('Ctrl Pts',(-38.3840553815676,42.1548781377002,-462.499999999991));
#32805=CARTESIAN_POINT('Ctrl Pts',(-38.0485358858946,42.4342626183073,-462.49999999999));
#32806=CARTESIAN_POINT('Ctrl Pts',(-37.7015139289768,42.6984598857191,-462.499999999992));
#32807=CARTESIAN_POINT('Ctrl Pts',(-37.6313113290433,42.751907037111,-462.499999999992));
#32808=CARTESIAN_POINT('Ctrl Pts',(-37.5606381983877,42.8047320086185,-462.499999999992));
#32809=CARTESIAN_POINT('Ctrl Pts',(-37.4895054223497,42.8569273733703,-462.499999999992));
#32810=CARTESIAN_POINT('Ctrl Pts',(-37.2083128059277,43.0632591376727,-462.499999999992));
#32811=CARTESIAN_POINT('Ctrl Pts',(-36.9199317767795,43.2597666774808,-462.499999999992));
#32812=CARTESIAN_POINT('Ctrl Pts',(-36.6250350054762,43.44599737661,-462.499999999992));
#32813=CARTESIAN_POINT('Ctrl Pts',(-36.4766084300011,43.5397304642866,-462.499999999992));
#32814=CARTESIAN_POINT('Ctrl Pts',(-36.3265298420472,43.6308599885747,-462.499999999992));
#32815=CARTESIAN_POINT('Ctrl Pts',(-36.1748926818072,43.719331120904,-462.499999999992));
#32816=CARTESIAN_POINT('Ctrl Pts',(-35.9475629882934,43.8519642786695,-462.499999999992));
#32817=CARTESIAN_POINT('Ctrl Pts',(-35.7167344653798,43.9786237267065,-462.499999999992));
#32818=CARTESIAN_POINT('Ctrl Pts',(-35.4827207341128,44.0991249603451,-462.499999999992));
#32819=CARTESIAN_POINT('Ctrl Pts',(-35.0926443215359,44.2999879125929,-462.499999999992));
#32820=CARTESIAN_POINT('Ctrl Pts',(-34.6937162549713,44.4837348679316,-462.499999999992));
#32821=CARTESIAN_POINT('Ctrl Pts',(-34.2872595209354,44.6497527723323,-462.499999999992));
#32822=CARTESIAN_POINT('Ctrl Pts',(-34.2870189837742,44.6498510128264,-462.499999999991));
#32823=CARTESIAN_POINT('Ctrl Pts',(-33.882499227078,44.8150532196688,-462.499999999992));
#32824=CARTESIAN_POINT('Ctrl Pts',(-33.4710017122312,44.9624982997247,-462.499999999992));
#32825=CARTESIAN_POINT('Ctrl Pts',(-33.0533836161765,45.091854154172,-462.499999999992));
#32826=CARTESIAN_POINT('Ctrl Pts',(-33.0529806979711,45.0919789381448,-462.499999999992));
#32827=CARTESIAN_POINT('Ctrl Pts',(-32.6383541991618,45.2203697961812,-462.499999999991));
#32828=CARTESIAN_POINT('Ctrl Pts',(-32.2184964333868,45.3306825375905,-462.499999999992));
#32829=CARTESIAN_POINT('Ctrl Pts',(-31.7948796623065,45.4225605594505,-462.499999999992));
#32830=CARTESIAN_POINT('',(-18.8785077902573,47.6382644181355,-462.499999999992));
#32831=CARTESIAN_POINT('Origin',(1.8061108164602E-11,-101.169000000086,
-462.499999999992));
#32832=CARTESIAN_POINT('',(-12.0150531445829,47.9060664143362,-462.499999999992));
#32833=CARTESIAN_POINT('Ctrl Pts',(-18.8785077902579,47.638264418134,-462.499999999996));
#32834=CARTESIAN_POINT('Ctrl Pts',(-18.5525168649589,47.5094378392464,-462.499999999996));
#32835=CARTESIAN_POINT('Ctrl Pts',(-17.4086215538667,47.057388076463,-462.499999999996));
#32836=CARTESIAN_POINT('Ctrl Pts',(-15.1447493101886,47.0351751898152,-462.499999999996));
#32837=CARTESIAN_POINT('Ctrl Pts',(-14.4547291834694,47.1123036398729,-462.499999999996));
#32838=CARTESIAN_POINT('Ctrl Pts',(-12.9164507181125,47.4785763558462,-462.499999999996));
#32839=CARTESIAN_POINT('Ctrl Pts',(-12.4871383760148,47.6751419616563,-462.499999999997));
#32840=CARTESIAN_POINT('Ctrl Pts',(-12.0150531445812,47.9060664143328,-462.499999999997));
#32841=CARTESIAN_POINT('',(-7.17826498482574,48.1389160151703,-462.499999999992));
#32842=CARTESIAN_POINT('Ctrl Pts',(-12.0150531445813,47.9060664143328,-462.499999999997));
#32843=CARTESIAN_POINT('Ctrl Pts',(-11.8254498398673,47.9988124619773,-462.499999999997));
#32844=CARTESIAN_POINT('Ctrl Pts',(-11.2182438109275,48.2958323869455,-462.499999999998));
#32845=CARTESIAN_POINT('Ctrl Pts',(-9.75062554367071,48.5431074753305,-462.499999999998));
#32846=CARTESIAN_POINT('Ctrl Pts',(-9.15039604630952,48.55483428605,-462.499999999998));
#32847=CARTESIAN_POINT('Ctrl Pts',(-7.88961170229352,48.3954373452753,-462.499999999998));
#32848=CARTESIAN_POINT('Ctrl Pts',(-7.55090612168781,48.2786384356784,-462.499999999997));
#32849=CARTESIAN_POINT('Ctrl Pts',(-7.17826498481883,48.1389160151649,-462.499999999997));
#32850=CARTESIAN_POINT('',(-2.51503960160435,48.2902113213028,-462.499999999992));
#32851=CARTESIAN_POINT('Ctrl Pts',(-7.17826498482668,48.1389160151678,-462.499999999997));
#32852=CARTESIAN_POINT('Ctrl Pts',(-6.93633745397943,48.0482048809024,-462.499999999997));
#32853=CARTESIAN_POINT('Ctrl Pts',(-6.04322837503661,47.7133321303008,-462.499999999995));
#32854=CARTESIAN_POINT('Ctrl Pts',(-3.62010262056583,47.7919488650083,-462.499999999995));
#32855=CARTESIAN_POINT('Ctrl Pts',(-2.75057840885255,48.1840091023979,-462.499999999997));
#32856=CARTESIAN_POINT('Ctrl Pts',(-2.51503960160297,48.2902113212998,-462.499999999997));
#32857=CARTESIAN_POINT('',(2.51503960159695,48.2902113215691,-462.499999999685));
#32858=CARTESIAN_POINT('Ctrl Pts',(-2.51503960160305,48.2902113212997,-462.499999999997));
#32859=CARTESIAN_POINT('Ctrl Pts',(-2.31486538455667,48.3804679811915,-462.499999999997));
#32860=CARTESIAN_POINT('Ctrl Pts',(-1.67033819224985,48.6710791924356,-462.5));
#32861=CARTESIAN_POINT('Ctrl Pts',(-0.126674917807384,48.8617608677135,
-462.5));
#32862=CARTESIAN_POINT('Ctrl Pts',(0.500972562625843,48.8421778966588,-462.5));
#32863=CARTESIAN_POINT('Ctrl Pts',(1.79880408278553,48.6019577853086,-462.5));
#32864=CARTESIAN_POINT('Ctrl Pts',(2.14046119294517,48.4591051805071,-462.499999999997));
#32865=CARTESIAN_POINT('Ctrl Pts',(2.51503960150293,48.290211321341,-462.499999999997));
#32866=CARTESIAN_POINT('',(7.17826498479954,48.1389160151653,-462.499999999992));
#32867=CARTESIAN_POINT('Ctrl Pts',(2.5150396014956,48.2902113213443,-462.499999999997));
#32868=CARTESIAN_POINT('Ctrl Pts',(3.01635259829434,48.0641740358177,-462.499999999997));
#32869=CARTESIAN_POINT('Ctrl Pts',(3.81474900505418,47.785633690015,-462.499999999995));
#32870=CARTESIAN_POINT('Ctrl Pts',(6.04322837400998,47.7133321303346,-462.499999999995));
#32871=CARTESIAN_POINT('Ctrl Pts',(6.93633745247155,48.0482048803425,-462.499999999997));
#32872=CARTESIAN_POINT('Ctrl Pts',(7.17826498480051,48.1389160151627,-462.499999999997));
#32873=CARTESIAN_POINT('Ctrl Pts',(7.17826498479326,48.13891601516,-462.499999999997));
#32874=CARTESIAN_POINT('Ctrl Pts',(7.57867402073054,48.289050056096,-462.499999999997));
#32875=CARTESIAN_POINT('Ctrl Pts',(7.94324496867089,48.4139972953879,-462.500000000092));
#32876=CARTESIAN_POINT('Ctrl Pts',(9.18080504777323,48.548614052163,-462.500000000092));
#32877=CARTESIAN_POINT('Ctrl Pts',(9.70223236095501,48.5392006175157,-462.500000000092));
#32878=CARTESIAN_POINT('Ctrl Pts',(11.0123813546909,48.3457034074005,-462.500000000092));
#32879=CARTESIAN_POINT('Ctrl Pts',(11.6260991509692,48.0963265243883,-462.499999999997));
#32880=CARTESIAN_POINT('Ctrl Pts',(12.0150531445265,47.9060664143568,-462.499999999997));
#32881=CARTESIAN_POINT('Origin',(3.88578058618805E-13,-3.17499999995531,
41.5000000000138));
#32882=CARTESIAN_POINT('Origin',(35.6399999999924,86.8310000000046,-333.499999999996));
#32883=CARTESIAN_POINT('Origin',(35.6399999999924,86.831,-377.5));
#32884=CARTESIAN_POINT('Origin',(47.999999999991,104.331000000009,-307.5));
#32885=CARTESIAN_POINT('',(47.999999999991,104.331000000009,-300.5));
#32886=CARTESIAN_POINT('',(54.999999999991,104.331000000009,-307.5));
#32887=CARTESIAN_POINT('Origin',(47.999999999991,104.331000000009,-307.5));
#32888=CARTESIAN_POINT('',(54.999999999991,104.331000000009,-307.5));
#32889=CARTESIAN_POINT('',(47.999999999991,104.331000000009,-300.5));
#32890=CARTESIAN_POINT('Origin',(54.999999999991,104.331000000004,-355.5));
#32891=CARTESIAN_POINT('',(54.999999999991,104.330999999998,-403.5));
#32892=CARTESIAN_POINT('',(54.999999999991,104.331000000004,-355.5));
#32893=CARTESIAN_POINT('',(54.999999999991,104.330999999998,-403.5));
#32894=CARTESIAN_POINT('Origin',(47.999999999991,104.330999999998,-403.5));
#32895=CARTESIAN_POINT('',(47.999999999991,104.330999999997,-410.5));
#32896=CARTESIAN_POINT('Origin',(47.999999999991,104.330999999998,-403.5));
#32897=CARTESIAN_POINT('',(47.999999999991,104.330999999997,-410.5));
#32898=CARTESIAN_POINT('Origin',(-1.500000000009,104.330999999992,-410.5));
#32899=CARTESIAN_POINT('',(-51.000000000009,104.330999999988,-410.5));
#32900=CARTESIAN_POINT('',(-1.50000000000897,104.330999999992,-410.5));
#32901=CARTESIAN_POINT('',(-51.000000000009,104.330999999988,-410.5));
#32902=CARTESIAN_POINT('Origin',(-51.000000000009,104.330999999989,-403.5));
#32903=CARTESIAN_POINT('',(-58.000000000009,104.330999999988,-403.5));
#32904=CARTESIAN_POINT('Origin',(-51.000000000009,104.330999999989,-403.5));
#32905=CARTESIAN_POINT('',(-58.000000000009,104.330999999988,-403.5));
#32906=CARTESIAN_POINT('Origin',(-58.000000000009,104.330999999994,-355.5));
#32907=CARTESIAN_POINT('',(-58.000000000009,104.331,-307.5));
#32908=CARTESIAN_POINT('',(-58.000000000009,104.330999999994,-355.5));
#32909=CARTESIAN_POINT('',(-58.000000000009,104.331,-307.5));
#32910=CARTESIAN_POINT('Origin',(-51.000000000009,104.331,-307.5));
#32911=CARTESIAN_POINT('',(-51.000000000009,104.331,-300.5));
#32912=CARTESIAN_POINT('Origin',(-51.000000000009,104.331,-307.5));
#32913=CARTESIAN_POINT('',(-51.000000000009,104.331,-300.5));
#32914=CARTESIAN_POINT('Origin',(-26.250000000009,104.331000000003,-300.5));
#32915=CARTESIAN_POINT('',(-1.50000000000897,104.331000000005,-300.5));
#32916=CARTESIAN_POINT('Ctrl Pts',(-64.2657293397397,-67.9791674266158,
-441.000046512357));
#32917=CARTESIAN_POINT('Ctrl Pts',(-52.7947107433608,-50.1279378633292,
-462.499360694393));
#32918=CARTESIAN_POINT('Ctrl Pts',(-67.6327997693264,-64.1661639590615,
-440.999999999978));
#32919=CARTESIAN_POINT('Ctrl Pts',(-54.7064708585543,-48.1213181445082,
-462.49999999998));
#32920=CARTESIAN_POINT('Ctrl Pts',(-69.5425906597941,-59.4517471898053,
-440.999999999979));
#32921=CARTESIAN_POINT('Ctrl Pts',(-56.0041009291202,-45.6723857139965,
-462.49999999998));
#32922=CARTESIAN_POINT('Ctrl Pts',(-69.7777140088065,-54.3725409130246,
-441.000032808645));
#32923=CARTESIAN_POINT('Ctrl Pts',(-56.5915605594633,-42.9638796623204,
-462.499999999981));
#32924=CARTESIAN_POINT('',(-64.2657293397398,-67.9791674266157,-441.000046512357));
#32925=CARTESIAN_POINT('',(-56.5915605594633,-42.9638796623205,-462.499999999981));
#32926=CARTESIAN_POINT('Ctrl Pts',(-56.8068436844474,-75.458414074715,-440.983703173492));
#32927=CARTESIAN_POINT('Ctrl Pts',(-56.7932797691753,-75.4496884498354,
-441.000046956267));
#32928=CARTESIAN_POINT('Ctrl Pts',(-44.7294130526197,-67.6890459439958,
-455.536347976562));
#32929=CARTESIAN_POINT('Ctrl Pts',(-44.7287959283668,-67.6886489496926,
-455.537091577965));
#32930=CARTESIAN_POINT('Ctrl Pts',(-56.8085894473236,-75.4568691036499,
-440.983703130936));
#32931=CARTESIAN_POINT('Ctrl Pts',(-56.79502657148,-75.4481423853249,-441.000046925264));
#32932=CARTESIAN_POINT('Ctrl Pts',(-44.7320913356736,-67.6865299469002,
-455.536351294835));
#32933=CARTESIAN_POINT('Ctrl Pts',(-44.7314742592658,-67.6861329032623,
-455.537094896055));
#32934=CARTESIAN_POINT('Ctrl Pts',(-56.8103352101999,-75.4553241325848,
-440.98370308838));
#32935=CARTESIAN_POINT('Ctrl Pts',(-56.7967733737847,-75.4465963208143,
-441.000046894262));
#32936=CARTESIAN_POINT('Ctrl Pts',(-44.7347696187276,-67.6840139498046,
-455.536354613108));
#32937=CARTESIAN_POINT('Ctrl Pts',(-44.7341525901647,-67.6836168568319,
-455.537098214144));
#32938=CARTESIAN_POINT('Ctrl Pts',(-56.8120809730762,-75.4537791615197,
-440.983703045824));
#32939=CARTESIAN_POINT('Ctrl Pts',(-56.7985201760894,-75.4450502563038,
-441.000046863259));
#32940=CARTESIAN_POINT('Ctrl Pts',(-44.7374479017815,-67.681497952709,-455.53635793138));
#32941=CARTESIAN_POINT('Ctrl Pts',(-44.7368309210637,-67.6811008104016,
-455.537101532234));
#32942=CARTESIAN_POINT('Ctrl Pts',(-59.4509723336889,-73.11840426527,-440.983638717812));
#32943=CARTESIAN_POINT('Ctrl Pts',(-59.4389827344453,-73.1080225102961,
-440.999999999977));
#32944=CARTESIAN_POINT('Ctrl Pts',(-48.7830207157301,-63.8810596701001,
-455.541370214754));
#32945=CARTESIAN_POINT('Ctrl Pts',(-48.7824760053808,-63.8805880071809,
-455.542113538993));
#32946=CARTESIAN_POINT('Ctrl Pts',(-61.940843357604,-70.6288920335432,-440.983638717812));
#32947=CARTESIAN_POINT('Ctrl Pts',(-61.9304681124401,-70.6168956516598,
-440.999999999977));
#32948=CARTESIAN_POINT('Ctrl Pts',(-52.7092909776335,-59.9549054455687,
-455.541370214755));
#32949=CARTESIAN_POINT('Ctrl Pts',(-52.7088196104674,-59.9543604270711,
-455.542113538993));
#32950=CARTESIAN_POINT('Ctrl Pts',(-64.2744496288301,-67.9927379636265,
-440.983702694819));
#32951=CARTESIAN_POINT('Ctrl Pts',(-64.2657293397397,-67.9791674266158,
-441.000046512357));
#32952=CARTESIAN_POINT('Ctrl Pts',(-56.5098402813215,-55.9094323036241,
-455.536357671384));
#32953=CARTESIAN_POINT('Ctrl Pts',(-56.5094435310252,-55.9088148797607,
-455.537101272242));
#32954=CARTESIAN_POINT('Ctrl Pts',(-64.2759934183429,-67.990994024618,-440.983702737144));
#32955=CARTESIAN_POINT('Ctrl Pts',(-64.267274224083,-67.9774224462302,-441.000046543128));
#32956=CARTESIAN_POINT('Ctrl Pts',(-56.512356333148,-55.9067541065334,-455.536354352964));
#32957=CARTESIAN_POINT('Ctrl Pts',(-56.5119596322498,-55.906136634736,-455.537097954005));
#32958=CARTESIAN_POINT('Ctrl Pts',(-64.2775372078555,-67.9892500856095,
-440.983702779468));
#32959=CARTESIAN_POINT('Ctrl Pts',(-64.2688191084264,-67.9756774658445,
-441.000046573897));
#32960=CARTESIAN_POINT('Ctrl Pts',(-56.5148723849746,-55.9040759094427,
-455.536351034544));
#32961=CARTESIAN_POINT('Ctrl Pts',(-56.5144757334745,-55.9034583897113,
-455.537094635768));
#32962=CARTESIAN_POINT('Ctrl Pts',(-64.2790809973682,-67.987506146601,-440.983702821791));
#32963=CARTESIAN_POINT('Ctrl Pts',(-64.2703639927698,-67.9739324854589,
-441.000046604668));
#32964=CARTESIAN_POINT('Ctrl Pts',(-56.5173884368011,-55.9013977123521,
-455.536347716124));
#32965=CARTESIAN_POINT('Ctrl Pts',(-56.5169918346991,-55.9007801446866,
-455.537091317531));
#32966=CARTESIAN_POINT('',(-56.7985201761028,-75.4450502562919,-441.000046863259));
#32967=CARTESIAN_POINT('Ctrl Pts',(-64.2657293397398,-67.9791674266157,
-441.000046512357));
#32968=CARTESIAN_POINT('Ctrl Pts',(-64.2379686007189,-68.0105725380733,
-441.000011935885));
#32969=CARTESIAN_POINT('Ctrl Pts',(-64.2006833472475,-68.0527069711186,
-440.999965951545));
#32970=CARTESIAN_POINT('Ctrl Pts',(-64.1198226715104,-68.1438289318397,
-440.999868753421));
#32971=CARTESIAN_POINT('Ctrl Pts',(-64.0832738799935,-68.1849360569023,
-440.999825609413));
#32972=CARTESIAN_POINT('Ctrl Pts',(-63.9735042890578,-68.3081570525,-440.999698381965));
#32973=CARTESIAN_POINT('Ctrl Pts',(-63.9001649872347,-68.3901652114701,
-440.99961650872));
#32974=CARTESIAN_POINT('Ctrl Pts',(-63.6796564581205,-68.6357853866767,
-440.999379598168));
#32975=CARTESIAN_POINT('Ctrl Pts',(-63.5320150171305,-68.7989722880318,
-440.999233289074));
#32976=CARTESIAN_POINT('Ctrl Pts',(-63.0871465110819,-69.2868934672009,
-440.998828453101));
#32977=CARTESIAN_POINT('Ctrl Pts',(-62.7880452046029,-69.6099093149823,
-440.99860404548));
#32978=CARTESIAN_POINT('Ctrl Pts',(-61.8831162212809,-70.5722204933488,
-440.998063183776));
#32979=CARTESIAN_POINT('Ctrl Pts',(-61.2699123367798,-71.2045014479794,
-440.997878501315));
#32980=CARTESIAN_POINT('Ctrl Pts',(-60.0244121795718,-72.4497779568237,
-440.997860569593));
#32981=CARTESIAN_POINT('Ctrl Pts',(-59.3921928542818,-73.0627068426545,
-440.998027192544));
#32982=CARTESIAN_POINT('Ctrl Pts',(-58.429873872212,-73.9673320492948,-440.998561014861));
#32983=CARTESIAN_POINT('Ctrl Pts',(-58.1067820084529,-74.2664003494679,
-440.998786485406));
#32984=CARTESIAN_POINT('Ctrl Pts',(-57.6187183951671,-74.7112440254951,
-440.999200642983));
#32985=CARTESIAN_POINT('Ctrl Pts',(-57.4554648297677,-74.8588940789512,
-440.999351364043));
#32986=CARTESIAN_POINT('Ctrl Pts',(-57.2097371052446,-75.0794213981712,
-440.999597178664));
#32987=CARTESIAN_POINT('Ctrl Pts',(-57.1276881746811,-75.1527711803181,
-440.99968240501));
#32988=CARTESIAN_POINT('Ctrl Pts',(-57.0044040747093,-75.2625579230306,
-440.999815278954));
#32989=CARTESIAN_POINT('Ctrl Pts',(-56.9632746672463,-75.2991134864768,
-440.999860408936));
#32990=CARTESIAN_POINT('Ctrl Pts',(-56.8721271094273,-75.3799679631664,
-440.999962214462));
#32991=CARTESIAN_POINT('Ctrl Pts',(-56.8299684290529,-75.4172613726013,
-441.000010497298));
#32992=CARTESIAN_POINT('Ctrl Pts',(-56.7985201761028,-75.4450502562919,
-441.000046863259));
#32993=CARTESIAN_POINT('Ctrl Pts',(-43.1946805031653,-80.9544448157854,
-441.000060157993));
#32994=CARTESIAN_POINT('Ctrl Pts',(-31.7948796622966,-67.7605605594826,
-462.499999999979));
#32995=CARTESIAN_POINT('Ctrl Pts',(-48.2746526175946,-80.7177558649757,
-440.999999999976));
#32996=CARTESIAN_POINT('Ctrl Pts',(-34.5033857139727,-67.17310092914,-462.499999999979));
#32997=CARTESIAN_POINT('Ctrl Pts',(-52.9882277635993,-78.8087212294075,
-440.999999999977));
#32998=CARTESIAN_POINT('Ctrl Pts',(-36.9523181444846,-65.8754708585745,
-462.499999999979));
#32999=CARTESIAN_POINT('Ctrl Pts',(-56.7985201760894,-75.4450502563038,
-441.000046863259));
#33000=CARTESIAN_POINT('Ctrl Pts',(-38.9600894847066,-63.9626889424092,
-462.499377237841));
#33001=CARTESIAN_POINT('',(-43.1946805031654,-80.9544448157855,-441.000060157993));
#33002=CARTESIAN_POINT('Ctrl Pts',(-30.0724252391789,-81.4699528747219,
-440.991833214076));
#33003=CARTESIAN_POINT('Ctrl Pts',(-30.0694361726661,-81.4653775066517,
-441.00006022933));
#33004=CARTESIAN_POINT('Ctrl Pts',(-22.2580066308467,-69.5084119606299,
-462.499999999978));
#33005=CARTESIAN_POINT('Ctrl Pts',(-22.2501512995082,-69.4963877945455,
-462.521620773711));
#33006=CARTESIAN_POINT('Ctrl Pts',(-34.4491834215995,-81.3268370384189,
-440.991760309822));
#33007=CARTESIAN_POINT('Ctrl Pts',(-34.4457390924923,-81.3221254984248,
-440.999999999977));
#33008=CARTESIAN_POINT('Ctrl Pts',(-25.4583773817378,-69.0282032793835,
-462.499999999979));
#33009=CARTESIAN_POINT('Ctrl Pts',(-25.4493533867006,-69.0158592459884,
-462.521587635987));
#33010=CARTESIAN_POINT('Ctrl Pts',(-38.8247825005319,-81.1566899975232,
-440.991744896788));
#33011=CARTESIAN_POINT('Ctrl Pts',(-38.8208728590296,-81.1518111816476,
-440.999999999977));
#33012=CARTESIAN_POINT('Ctrl Pts',(-28.6384087051628,-68.4451812419869,
-462.499999999979));
#33013=CARTESIAN_POINT('Ctrl Pts',(-28.628203825419,-68.4324466397802,-462.521547329895));
#33014=CARTESIAN_POINT('Ctrl Pts',(-43.1990671867739,-80.959521869026,-440.99178690524));
#33015=CARTESIAN_POINT('Ctrl Pts',(-43.1946805031653,-80.9544448157854,
-441.000060157993));
#33016=CARTESIAN_POINT('Ctrl Pts',(-31.7948796622966,-67.7605605594826,
-462.499999999979));
#33017=CARTESIAN_POINT('Ctrl Pts',(-31.7834798614557,-67.7473666752263,
-462.521499939821));
#33018=CARTESIAN_POINT('',(-30.0769139794115,-81.465138787044,-441.000049420363));
#33019=CARTESIAN_POINT('Ctrl Pts',(-25.9994431732858,-68.8985804999237,
-462.499999999979));
#33020=CARTESIAN_POINT('Ctrl Pts',(-26.7964799308327,-70.6751920159385,
-459.557188447894));
#33021=CARTESIAN_POINT('Ctrl Pts',(-27.479108889254,-72.495769348422,-456.514213204788));
#33022=CARTESIAN_POINT('Ctrl Pts',(-28.4752491269335,-75.495938283277,-451.414006370867));
#33023=CARTESIAN_POINT('Ctrl Pts',(-28.8452960300499,-76.7249502701369,
-449.301561414758));
#33024=CARTESIAN_POINT('Ctrl Pts',(-29.5081306533979,-79.1196286730972,
-445.139987269977));
#33025=CARTESIAN_POINT('Ctrl Pts',(-29.8061604421476,-80.2987054845064,
-443.068993354753));
#33026=CARTESIAN_POINT('Ctrl Pts',(-30.0769139781574,-81.4651387869444,
-441.000049420142));
#33027=CARTESIAN_POINT('Ctrl Pts',(-43.1946805031653,-80.9544448157855,
-441.000060157993));
#33028=CARTESIAN_POINT('Ctrl Pts',(-40.9465691514988,-81.0577146082457,
-440.997167465374));
#33029=CARTESIAN_POINT('Ctrl Pts',(-38.6981106838266,-81.1529027064473,
-440.995568194053));
#33030=CARTESIAN_POINT('Ctrl Pts',(-34.3253844906309,-81.3222673217518,
-440.995559720608));
#33031=CARTESIAN_POINT('Ctrl Pts',(-32.2013690465366,-81.3973097918519,
-440.99698028376));
#33032=CARTESIAN_POINT('Ctrl Pts',(-30.076913979416,-81.465138787221,-441.000049419583));
#33033=CARTESIAN_POINT('Origin',(5.02375918642883E-12,-65.4426315587606,
-438.999999999979));
#33034=CARTESIAN_POINT('',(-25.7039045353314,-81.6296264484025,-438.999999999976));
#33035=CARTESIAN_POINT('',(-23.5144780620957,-81.6868555254876,-438.999999999977));
#33036=CARTESIAN_POINT('Origin',(0.000161522130812664,859.827648708006,
-438.999999684644));
#33037=CARTESIAN_POINT('Ctrl Pts',(-25.7039045353315,-81.6296264484023,
-438.999999999977));
#33038=CARTESIAN_POINT('Ctrl Pts',(-25.338907423015,-81.6125050746809,-438.999999999977));
#33039=CARTESIAN_POINT('Ctrl Pts',(-24.9734197856892,-81.608705495081,-438.999999999974));
#33040=CARTESIAN_POINT('Ctrl Pts',(-24.2428714081309,-81.6277925001813,
-438.999999999974));
#33041=CARTESIAN_POINT('Ctrl Pts',(-23.8780813890794,-81.6506720610301,
-438.999999999977));
#33042=CARTESIAN_POINT('Ctrl Pts',(-23.5144780620957,-81.6868555254874,
-438.999999999977));
#33043=CARTESIAN_POINT('Ctrl Pts',(-18.2815673778157,-69.4842526335149,
-462.499999999979));
#33044=CARTESIAN_POINT('Ctrl Pts',(-20.9895259839786,-82.1584973191859,
-439.001498361858));
#33045=CARTESIAN_POINT('Ctrl Pts',(-20.8066529721932,-68.4044021024295,
-462.499999999979));
#33046=CARTESIAN_POINT('Ctrl Pts',(-24.0993037835529,-81.2970472206573,
-438.998064517714));
#33047=CARTESIAN_POINT('Ctrl Pts',(-23.6668225473958,-68.1714685993807,
-462.499999999979));
#33048=CARTESIAN_POINT('Ctrl Pts',(-27.4436430653255,-81.41563992135,-439.00145091813));
#33049=CARTESIAN_POINT('Ctrl Pts',(-26.5149982528597,-69.0440180664332,
-462.499999999978));
#33050=CARTESIAN_POINT('Ctrl Pts',(-30.6502301549084,-82.7145147968836,
-438.999999999977));
#33051=CARTESIAN_POINT('Ctrl Pts',(-30.0769139793183,-81.4651387872084,
-441.000049420484));
#33052=CARTESIAN_POINT('Ctrl Pts',(-29.551680891548,-81.4895072998655,-440.565682691273));
#33053=CARTESIAN_POINT('Ctrl Pts',(-28.9861515269315,-81.513823687901,-440.18289056592));
#33054=CARTESIAN_POINT('Ctrl Pts',(-27.540804130675,-81.5705690446153,-439.428837284769));
#33055=CARTESIAN_POINT('Ctrl Pts',(-26.6435506045776,-81.6016843613183,
-439.131000321948));
#33056=CARTESIAN_POINT('Ctrl Pts',(-25.7039045353331,-81.6296264484023,
-438.999999999977));
#33057=CARTESIAN_POINT('',(-20.8989998873753,-81.7348018106293,-439.787044944617));
#33058=CARTESIAN_POINT('',(-18.2815673778157,-69.4842526335148,-462.499999999978));
#33059=CARTESIAN_POINT('Ctrl Pts',(-23.5144780620922,-81.6868555254877,
-438.999999999977));
#33060=CARTESIAN_POINT('Ctrl Pts',(-23.0030694413233,-81.6984039047958,
-439.070113764198));
#33061=CARTESIAN_POINT('Ctrl Pts',(-22.5005158148452,-81.7084840649418,
-439.187699311006));
#33062=CARTESIAN_POINT('Ctrl Pts',(-21.6305049523498,-81.7238853085043,
-439.470420490408));
#33063=CARTESIAN_POINT('Ctrl Pts',(-21.2600040239069,-81.729739132405,-439.618066172395));
#33064=CARTESIAN_POINT('Ctrl Pts',(-20.8989998873755,-81.7348018106293,
-439.787044944617));
#33065=CARTESIAN_POINT('Ctrl Pts',(-10.4654930467012,-70.2592650976151,
-462.499999999978));
#33066=CARTESIAN_POINT('Ctrl Pts',(-12.3200202973713,-81.9438009571564,
-439.788405446002));
#33067=CARTESIAN_POINT('Ctrl Pts',(-13.1095347614995,-70.8130060900615,
-462.499999999978));
#33068=CARTESIAN_POINT('Ctrl Pts',(-15.1681070338602,-82.5994409013717,
-439.778955852854));
#33069=CARTESIAN_POINT('Ctrl Pts',(-15.7977562350973,-70.5464521833251,
-462.499999999978));
#33070=CARTESIAN_POINT('Ctrl Pts',(-18.0885677400365,-82.5280608755568,
-439.778955852854));
#33071=CARTESIAN_POINT('Ctrl Pts',(-18.2815673778157,-69.4842526335149,
-462.499999999979));
#33072=CARTESIAN_POINT('Ctrl Pts',(-20.8989998873753,-81.7348018106291,
-439.787044944617));
#33073=CARTESIAN_POINT('',(-12.3105614915023,-81.8842053074701,-439.904243357679));
#33074=CARTESIAN_POINT('',(-10.4654930467012,-70.2592650976151,-462.499999999978));
#33075=CARTESIAN_POINT('Ctrl Pts',(-20.8989998873751,-81.7348018106294,
-439.787044944617));
#33076=CARTESIAN_POINT('Ctrl Pts',(-19.6456374495956,-81.7524189300427,
-440.37142096878));
#33077=CARTESIAN_POINT('Ctrl Pts',(-18.3143448116165,-81.7724261674984,
-440.772667881321));
#33078=CARTESIAN_POINT('Ctrl Pts',(-16.1385805324535,-81.809038794424,-440.916888546948));
#33079=CARTESIAN_POINT('Ctrl Pts',(-15.3491371083455,-81.8231310310214,
-440.865014920264));
#33080=CARTESIAN_POINT('Ctrl Pts',(-13.7808037670599,-81.8531011884192,
-440.538114526936));
#33081=CARTESIAN_POINT('Ctrl Pts',(-13.0285402685663,-81.8684908169203,
-440.266775657381));
#33082=CARTESIAN_POINT('Ctrl Pts',(-12.3105614915036,-81.8842053074704,
-439.904243357677));
#33083=CARTESIAN_POINT('Origin',(5.02375918642883E-12,-65.4426315587606,
-438.999999999979));
#33084=CARTESIAN_POINT('',(-9.48352202361111,-81.9327028027076,-438.999999999976));
#33085=CARTESIAN_POINT('',(-7.12117861053857,-81.9535288684061,-438.999999999977));
#33086=CARTESIAN_POINT('Origin',(0.000159838139652813,859.827666094174,
-438.999999728954));
#33087=CARTESIAN_POINT('Ctrl Pts',(-9.48352202361107,-81.9327028027073,
-438.999999999977));
#33088=CARTESIAN_POINT('Ctrl Pts',(-9.08970639030352,-81.9095180552699,
-438.999999999977));
#33089=CARTESIAN_POINT('Ctrl Pts',(-8.69522724576118,-81.8996692479367,
-438.999999999977));
#33090=CARTESIAN_POINT('Ctrl Pts',(-7.90709887115381,-81.9066737233761,
-438.999999999977));
#33091=CARTESIAN_POINT('Ctrl Pts',(-7.51369125012755,-81.9234683536681,
-438.999999999977));
#33092=CARTESIAN_POINT('Ctrl Pts',(-7.12117861053855,-81.9535288684059,
-438.999999999977));
#33093=CARTESIAN_POINT('Ctrl Pts',(-3.89356335293881,-70.5754050032805,
-462.499999999978));
#33094=CARTESIAN_POINT('Ctrl Pts',(-4.22808633459723,-82.4205871416874,
-439.001458640508));
#33095=CARTESIAN_POINT('Ctrl Pts',(-6.03305280327815,-69.9075280596242,
-462.499999999979));
#33096=CARTESIAN_POINT('Ctrl Pts',(-6.91662420919795,-81.7519577109097,
-438.999332051806));
#33097=CARTESIAN_POINT('Ctrl Pts',(-8.27177497984179,-69.7998352736863,
-462.499999999979));
#33098=CARTESIAN_POINT('Ctrl Pts',(-9.68449268817595,-81.7275714335143,
-438.99931906013));
#33099=CARTESIAN_POINT('Ctrl Pts',(-10.4654930467012,-70.2592650976151,
-462.499999999978));
#33100=CARTESIAN_POINT('Ctrl Pts',(-12.3842779267235,-82.3486591624718,
-439.001470002309));
#33101=CARTESIAN_POINT('',(-4.21493383398708,-81.95486797187,-439.925355043788));
#33102=CARTESIAN_POINT('',(-3.89356335293881,-70.5754050032805,-462.499999999978));
#33103=CARTESIAN_POINT('Ctrl Pts',(-7.12117861053848,-81.9535288684062,
-438.999999999976));
#33104=CARTESIAN_POINT('Ctrl Pts',(-6.62324952873175,-81.9560718440252,
-439.070014738437));
#33105=CARTESIAN_POINT('Ctrl Pts',(-6.13364118294728,-81.9574020359696,
-439.183225075406));
#33106=CARTESIAN_POINT('Ctrl Pts',(-5.15947229064142,-81.9578371438549,
-439.493384596533));
#33107=CARTESIAN_POINT('Ctrl Pts',(-4.67905024494302,-81.9568662510572,
-439.691871923607));
#33108=CARTESIAN_POINT('Ctrl Pts',(-4.21493383398643,-81.9548679718702,
-439.925355043786));
#33109=CARTESIAN_POINT('Ctrl Pts',(-12.3105614915033,-81.8842053074704,
-439.904243357676));
#33110=CARTESIAN_POINT('Ctrl Pts',(-11.8610189703665,-81.8940670193849,
-439.675963799339));
#33111=CARTESIAN_POINT('Ctrl Pts',(-11.3953934000695,-81.9032084453796,
-439.482522031307));
#33112=CARTESIAN_POINT('Ctrl Pts',(-10.4475434646805,-81.9194866185534,
-439.179364695647));
#33113=CARTESIAN_POINT('Ctrl Pts',(-9.96967424536579,-81.9266070176389,
-439.068753183443));
#33114=CARTESIAN_POINT('Ctrl Pts',(-9.48352202361117,-81.9327028027076,
-438.999999999976));
#33115=CARTESIAN_POINT('Ctrl Pts',(3.89356335294888,-70.5754050032799,-462.499999999978));
#33116=CARTESIAN_POINT('Ctrl Pts',(4.21493383919102,-81.9548693923795,-439.925355068582));
#33117=CARTESIAN_POINT('Ctrl Pts',(1.33838929652316,-71.3730447574958,-462.499999999978));
#33118=CARTESIAN_POINT('Ctrl Pts',(1.43390756316856,-82.6552216731943,-439.915749851982));
#33119=CARTESIAN_POINT('Ctrl Pts',(-1.33838929651297,-71.3730447574961,
-462.499999999978));
#33120=CARTESIAN_POINT('Ctrl Pts',(-1.43390756315624,-82.6552216731946,
-439.915749851982));
#33121=CARTESIAN_POINT('Ctrl Pts',(-3.89356335293881,-70.5754050032805,
-462.499999999978));
#33122=CARTESIAN_POINT('Ctrl Pts',(-4.21493383398708,-81.95486797187,-439.925355043787));
#33123=CARTESIAN_POINT('',(4.21493383919094,-81.9548693923797,-439.925355068582));
#33124=CARTESIAN_POINT('',(3.89356335294888,-70.5754050032799,-462.499999999978));
#33125=CARTESIAN_POINT('Ctrl Pts',(4.21493383919057,-81.9548693923798,-439.925355068582));
#33126=CARTESIAN_POINT('Ctrl Pts',(3.54934499941135,-81.9520270095361,-440.25884255782));
#33127=CARTESIAN_POINT('Ctrl Pts',(2.8548204219887,-81.9497427021224,-440.52735679615));
#33128=CARTESIAN_POINT('Ctrl Pts',(1.43300534097921,-81.9466845475377,-440.88703829099));
#33129=CARTESIAN_POINT('Ctrl Pts',(0.721578194027332,-81.9458978792099,
-440.979675755148));
#33130=CARTESIAN_POINT('Ctrl Pts',(-0.722493479587384,-81.9458984309402,
-440.979581995565));
#33131=CARTESIAN_POINT('Ctrl Pts',(-1.43373571979195,-81.9466852459727,
-440.886898928913));
#33132=CARTESIAN_POINT('Ctrl Pts',(-2.85517004898937,-81.9497428822133,
-440.527222128221));
#33133=CARTESIAN_POINT('Ctrl Pts',(-3.54951323389898,-81.9520265269081,
-440.258758519013));
#33134=CARTESIAN_POINT('Ctrl Pts',(-4.2149338339865,-81.9548679718702,-439.925355043787));
#33135=CARTESIAN_POINT('Origin',(5.02375918642883E-12,-65.4426315587606,
-438.999999999979));
#33136=CARTESIAN_POINT('',(7.12117862753353,-81.9535312690186,-438.999999999978));
#33137=CARTESIAN_POINT('',(9.48352205464678,-81.9327059996163,-438.999999999978));
#33138=CARTESIAN_POINT('Origin',(0.000157662688085036,859.827665975351,
-439.000000180659));
#33139=CARTESIAN_POINT('Ctrl Pts',(7.12117862753352,-81.9535312690185,-438.999999999978));
#33140=CARTESIAN_POINT('Ctrl Pts',(7.51410779327789,-81.9234389742552,-438.999999999978));
#33141=CARTESIAN_POINT('Ctrl Pts',(7.90793370256448,-81.9066407489514,-438.999999999977));
#33142=CARTESIAN_POINT('Ctrl Pts',(8.69606258685533,-81.8996930223353,-438.999999999977));
#33143=CARTESIAN_POINT('Ctrl Pts',(9.09012343726988,-81.9095456552935,-438.999999999978));
#33144=CARTESIAN_POINT('Ctrl Pts',(9.48352205464679,-81.9327059996161,-438.999999999978));
#33145=CARTESIAN_POINT('Ctrl Pts',(10.4654930467115,-70.2592650976135,-462.499999999978));
#33146=CARTESIAN_POINT('Ctrl Pts',(12.3842778439454,-82.3486626074551,-439.001471767375));
#33147=CARTESIAN_POINT('Ctrl Pts',(8.27177497985184,-69.7998352736849,-462.499999999978));
#33148=CARTESIAN_POINT('Ctrl Pts',(9.68449198910565,-81.7275751837853,-438.999317851236));
#33149=CARTESIAN_POINT('Ctrl Pts',(6.03305280328818,-69.9075280596233,-462.499999999978));
#33150=CARTESIAN_POINT('Ctrl Pts',(6.91662493113332,-81.7519599718325,-438.999332171566));
#33151=CARTESIAN_POINT('Ctrl Pts',(3.89356335294888,-70.5754050032799,-462.499999999978));
#33152=CARTESIAN_POINT('Ctrl Pts',(4.22808633184835,-82.4205883312023,-439.001459239898));
#33153=CARTESIAN_POINT('',(12.3105615445815,-81.8842094560395,-439.904243430097));
#33154=CARTESIAN_POINT('',(10.4654930467115,-70.2592650976135,-462.499999999979));
#33155=CARTESIAN_POINT('Ctrl Pts',(9.48352205464689,-81.9327059996164,-438.999999999977));
#33156=CARTESIAN_POINT('Ctrl Pts',(9.96970255654653,-81.9266100234847,-439.068757204431));
#33157=CARTESIAN_POINT('Ctrl Pts',(10.4475989576107,-81.919489312792,-439.179377597763));
#33158=CARTESIAN_POINT('Ctrl Pts',(11.3954460472368,-81.9032112524941,-439.482543979102));
#33159=CARTESIAN_POINT('Ctrl Pts',(11.8610444462678,-81.8940704579246,-439.675976824542));
#33160=CARTESIAN_POINT('Ctrl Pts',(12.3105615445817,-81.8842094560397,-439.904243430096));
#33161=CARTESIAN_POINT('Ctrl Pts',(4.21493383919116,-81.9548693923798,-439.925355068582));
#33162=CARTESIAN_POINT('Ctrl Pts',(4.67904816069443,-81.956867818085,-439.691873053696));
#33163=CARTESIAN_POINT('Ctrl Pts',(5.15946796055897,-81.9578388730233,-439.49338646958));
#33164=CARTESIAN_POINT('Ctrl Pts',(6.13363661544826,-81.9574041152318,-439.183226185497));
#33165=CARTESIAN_POINT('Ctrl Pts',(6.62324720515649,-81.9560740883707,-439.070015088001));
#33166=CARTESIAN_POINT('Ctrl Pts',(7.12117862753345,-81.9535312690188,-438.999999999977));
#33167=CARTESIAN_POINT('Ctrl Pts',(18.2815673778257,-69.4842526335121,-462.499999999979));
#33168=CARTESIAN_POINT('Ctrl Pts',(20.8990000425199,-81.7348088522914,-439.787045067561));
#33169=CARTESIAN_POINT('Ctrl Pts',(15.7977562351075,-70.5464521833227,-462.499999999978));
#33170=CARTESIAN_POINT('Ctrl Pts',(18.0885677400489,-82.5280608755536,-439.778955852855));
#33171=CARTESIAN_POINT('Ctrl Pts',(13.1095347615097,-70.8130060900595,-462.499999999978));
#33172=CARTESIAN_POINT('Ctrl Pts',(15.1681070338725,-82.599440901369,-439.778955852855));
#33173=CARTESIAN_POINT('Ctrl Pts',(10.4654930467115,-70.2592650976135,-462.499999999978));
#33174=CARTESIAN_POINT('Ctrl Pts',(12.3200202173657,-81.9438042867714,-439.788407151959));
#33175=CARTESIAN_POINT('',(20.8990000425197,-81.7348088522915,-439.787045067561));
#33176=CARTESIAN_POINT('',(18.2815673778257,-69.4842526335121,-462.499999999979));
#33177=CARTESIAN_POINT('Ctrl Pts',(12.3105615445817,-81.8842094560396,-439.904243430097));
#33178=CARTESIAN_POINT('Ctrl Pts',(12.9424829255709,-81.8703787725802,-440.223319792049));
#33179=CARTESIAN_POINT('Ctrl Pts',(13.6020736939311,-81.8567751181056,-440.472315085927));
#33180=CARTESIAN_POINT('Ctrl Pts',(14.9703535636644,-81.8302081245194,-440.804754741935));
#33181=CARTESIAN_POINT('Ctrl Pts',(15.6610816623562,-81.8175741397569,-440.885758233786));
#33182=CARTESIAN_POINT('Ctrl Pts',(17.1296347509788,-81.7921241598419,-440.881946716635));
#33183=CARTESIAN_POINT('Ctrl Pts',(17.8889355257091,-81.7797619763488,-440.780290522576));
#33184=CARTESIAN_POINT('Ctrl Pts',(19.4146607479418,-81.7561159296533,-440.405153968589));
#33185=CARTESIAN_POINT('Ctrl Pts',(20.1714264871945,-81.7450353487284,-440.126270879395));
#33186=CARTESIAN_POINT('Ctrl Pts',(20.8990000425196,-81.7348088522916,-439.787045067561));
#33187=CARTESIAN_POINT('Origin',(5.02375918642883E-12,-65.4426315587606,
-438.999999999979));
#33188=CARTESIAN_POINT('',(23.5144782588677,-81.6868634501823,-438.999999999977));
#33189=CARTESIAN_POINT('',(25.7039047706638,-81.6296351104369,-438.999999999978));
#33190=CARTESIAN_POINT('Origin',(0.000155981030567354,859.827648586247,
-438.999999842311));
#33191=CARTESIAN_POINT('Ctrl Pts',(23.5144782588677,-81.686863450182,-438.999999999977));
#33192=CARTESIAN_POINT('Ctrl Pts',(23.8779552573195,-81.6506927118015,-438.999999999977));
#33193=CARTESIAN_POINT('Ctrl Pts',(24.2426281344593,-81.6278161321225,-438.999999999973));
#33194=CARTESIAN_POINT('Ctrl Pts',(24.9731693890883,-81.608711524059,-438.999999999973));
#33195=CARTESIAN_POINT('Ctrl Pts',(25.3387874851401,-81.6125080570722,-438.999999999977));
#33196=CARTESIAN_POINT('Ctrl Pts',(25.7039047706638,-81.6296351104367,-438.999999999977));
#33197=CARTESIAN_POINT('Ctrl Pts',(26.5149982231106,-69.0440180573124,-462.499999999979));
#33198=CARTESIAN_POINT('Ctrl Pts',(30.6502301216108,-82.7145147833341,-438.999999999977));
#33199=CARTESIAN_POINT('Ctrl Pts',(23.6668225265683,-68.171468601074,-462.499999999979));
#33200=CARTESIAN_POINT('Ctrl Pts',(27.4436392089424,-81.415652603698,-439.001453877264));
#33201=CARTESIAN_POINT('Ctrl Pts',(20.8066529626785,-68.4044021064994,-462.499999999979));
#33202=CARTESIAN_POINT('Ctrl Pts',(24.0993065058744,-81.29705577815,-438.998060570033));
#33203=CARTESIAN_POINT('Ctrl Pts',(18.2815673778257,-69.4842526335121,-462.499999999979));
#33204=CARTESIAN_POINT('Ctrl Pts',(20.9895258069676,-82.1585030246664,-439.001501417916));
#33205=CARTESIAN_POINT('',(30.0769364718121,-81.4651482118546,-441.000049527067));
#33206=CARTESIAN_POINT('Ctrl Pts',(30.0769364733382,-81.4651482119768,-441.000049527336));
#33207=CARTESIAN_POINT('Ctrl Pts',(29.8061861881463,-80.2987458269529,-443.068934798007));
#33208=CARTESIAN_POINT('Ctrl Pts',(29.5081626488663,-79.1197036090261,-445.139865574628));
#33209=CARTESIAN_POINT('Ctrl Pts',(28.8453460499946,-76.7250958481571,-449.301315287558));
#33210=CARTESIAN_POINT('Ctrl Pts',(28.4753114889536,-75.4961210030392,-451.41369731436));
#33211=CARTESIAN_POINT('Ctrl Pts',(27.4791729678182,-72.4959292673654,-456.513948240452));
#33212=CARTESIAN_POINT('Ctrl Pts',(26.7965164718484,-70.6752595300762,-459.55708022097));
#33213=CARTESIAN_POINT('Ctrl Pts',(25.9994431732941,-68.8985804999194,-462.499999999979));
#33214=CARTESIAN_POINT('Ctrl Pts',(25.7039047706639,-81.6296351104371,-438.999999999977));
#33215=CARTESIAN_POINT('Ctrl Pts',(26.6066393041569,-81.6027909675482,-439.125853859304));
#33216=CARTESIAN_POINT('Ctrl Pts',(27.4708379293598,-81.5730007420501,-439.405781130766));
#33217=CARTESIAN_POINT('Ctrl Pts',(28.9250644802948,-81.5164546086103,-440.141784715098));
#33218=CARTESIAN_POINT('Ctrl Pts',(29.5233073521062,-81.4908339430079,-440.542202709549));
#33219=CARTESIAN_POINT('Ctrl Pts',(30.0769364719202,-81.4651482116506,-441.000049526925));
#33220=CARTESIAN_POINT('Ctrl Pts',(20.8990000425198,-81.7348088522916,-439.787045067561));
#33221=CARTESIAN_POINT('Ctrl Pts',(21.3204957294972,-81.7288979936655,-439.58975120819));
#33222=CARTESIAN_POINT('Ctrl Pts',(21.7548089567099,-81.7219103005923,-439.421599055221));
#33223=CARTESIAN_POINT('Ctrl Pts',(22.6307047917946,-81.7058594459475,-439.158050593173));
#33224=CARTESIAN_POINT('Ctrl Pts',(23.0693369665686,-81.6969152647404,-439.061028459663));
#33225=CARTESIAN_POINT('Ctrl Pts',(23.5144782588676,-81.6868634501824,-438.999999999977));
#33226=CARTESIAN_POINT('Ctrl Pts',(43.201920988198,-80.9594167953459,-440.991769323448));
#33227=CARTESIAN_POINT('Ctrl Pts',(43.197523751011,-80.9543288413526,-441.000060412176));
#33228=CARTESIAN_POINT('Ctrl Pts',(31.7948796623075,-67.7605605594772,-462.499999999979));
#33229=CARTESIAN_POINT('Ctrl Pts',(31.7834770182188,-67.7473667911953,-462.521499939567));
#33230=CARTESIAN_POINT('Ctrl Pts',(38.8247909292306,-81.1567005156185,-440.991727099844));
#33231=CARTESIAN_POINT('Ctrl Pts',(38.8208728590421,-81.151811181641,-440.999999999977));
#33232=CARTESIAN_POINT('Ctrl Pts',(28.638408705173,-68.4451812419819,-462.499999999979));
#33233=CARTESIAN_POINT('Ctrl Pts',(28.6282038254292,-68.4324466397753,-462.521547329896));
#33234=CARTESIAN_POINT('Ctrl Pts',(34.4491908471433,-81.3268471958895,-440.991742546106));
#33235=CARTESIAN_POINT('Ctrl Pts',(34.4457390925038,-81.3221254984189,-440.999999999977));
#33236=CARTESIAN_POINT('Ctrl Pts',(25.4583773817474,-69.0282032793794,-462.499999999978));
#33237=CARTESIAN_POINT('Ctrl Pts',(25.4493533867103,-69.0158592459841,-462.521587635989));
#33238=CARTESIAN_POINT('Ctrl Pts',(30.0724320076141,-81.4699728715382,-440.991815654647));
#33239=CARTESIAN_POINT('Ctrl Pts',(30.0694364969325,-81.4653876356763,-441.000060406224));
#33240=CARTESIAN_POINT('Ctrl Pts',(22.2580066308556,-69.5084119606264,-462.499999999979));
#33241=CARTESIAN_POINT('Ctrl Pts',(22.250151299191,-69.496387784356,-462.521620773535));
#33242=CARTESIAN_POINT('Ctrl Pts',(30.0769364718065,-81.465148211635,-441.000049528026));
#33243=CARTESIAN_POINT('Ctrl Pts',(32.2034419211209,-81.3972545994429,-440.996967120045));
#33244=CARTESIAN_POINT('Ctrl Pts',(34.329571566688,-81.3221311807446,-440.995540157727));
#33245=CARTESIAN_POINT('Ctrl Pts',(38.703204763265,-81.1527038540004,-440.995547974776));
#33246=CARTESIAN_POINT('Ctrl Pts',(40.9505527826719,-81.0575526448392,-440.997149115757));
#33247=CARTESIAN_POINT('Ctrl Pts',(43.1975237510106,-80.9543288413528,-441.000060412176));
#33248=CARTESIAN_POINT('Ctrl Pts',(38.9588941886819,-63.9631388095498,-462.498954222077));
#33249=CARTESIAN_POINT('Ctrl Pts',(38.9383104029384,-63.9498936427278,-462.523755685796));
#33250=CARTESIAN_POINT('Ctrl Pts',(36.9523181444951,-65.8754708585682,-462.499999999979));
#33251=CARTESIAN_POINT('Ctrl Pts',(36.934067668895,-65.8607515207863,-462.52446915918));
#33252=CARTESIAN_POINT('Ctrl Pts',(34.5033857139835,-67.173100929134,-462.499999999979));
#33253=CARTESIAN_POINT('Ctrl Pts',(34.487712629227,-67.1576857515551,-462.52446915918));
#33254=CARTESIAN_POINT('Ctrl Pts',(31.7948796623075,-67.7605605594772,-462.499999999979));
#33255=CARTESIAN_POINT('Ctrl Pts',(31.7817253813645,-67.7453400077063,-462.524802689899));
#33256=CARTESIAN_POINT('Ctrl Pts',(64.2844510030596,-67.9859312604405,-440.982510346491));
#33257=CARTESIAN_POINT('Ctrl Pts',(64.2750751909262,-67.9713441846113,-441.000078299647));
#33258=CARTESIAN_POINT('Ctrl Pts',(56.5172406812969,-55.9015414418543,-455.536347698364));
#33259=CARTESIAN_POINT('Ctrl Pts',(56.5171259388062,-55.9013629232716,-455.536562697357));
#33260=CARTESIAN_POINT('Ctrl Pts',(64.2829289255942,-67.9876489086986,-440.982510283378));
#33261=CARTESIAN_POINT('Ctrl Pts',(64.2735519592642,-67.9730629321979,-441.000078248778));
#33262=CARTESIAN_POINT('Ctrl Pts',(56.5147649746143,-55.9041767025935,-455.536350963711));
#33263=CARTESIAN_POINT('Ctrl Pts',(56.5146502181162,-55.9039981976221,-455.536565962653));
#33264=CARTESIAN_POINT('Ctrl Pts',(64.2814068481288,-67.9893665569567,-440.982510220263));
#33265=CARTESIAN_POINT('Ctrl Pts',(64.2720287276024,-67.9747816797845,-441.000078197908));
#33266=CARTESIAN_POINT('Ctrl Pts',(56.5122892679318,-55.9068119633328,-455.536354229059));
#33267=CARTESIAN_POINT('Ctrl Pts',(56.5121744974262,-55.9066334719727,-455.536569227948));
#33268=CARTESIAN_POINT('Ctrl Pts',(64.2798847706634,-67.9910842052148,-440.982510157149));
#33269=CARTESIAN_POINT('Ctrl Pts',(64.2705054959406,-67.9765004273711,-441.000078147038));
#33270=CARTESIAN_POINT('Ctrl Pts',(56.5098135612492,-55.909447224072,-455.536357494406));
#33271=CARTESIAN_POINT('Ctrl Pts',(56.5096987767362,-55.9092687463232,-455.536572493243));
#33272=CARTESIAN_POINT('Ctrl Pts',(61.9416205008464,-70.629790605742,-440.982413198853));
#33273=CARTESIAN_POINT('Ctrl Pts',(61.9304681124519,-70.6168956516489,-440.999999999979));
#33274=CARTESIAN_POINT('Ctrl Pts',(52.7092909776432,-59.9549054455595,-455.541370214756));
#33275=CARTESIAN_POINT('Ctrl Pts',(52.7091546899917,-59.9547478629012,-455.541585134084));
#33276=CARTESIAN_POINT('Ctrl Pts',(59.4518703978667,-73.1191818960986,-440.982413198852));
#33277=CARTESIAN_POINT('Ctrl Pts',(59.4389827344574,-73.1080225102857,-440.999999999979));
#33278=CARTESIAN_POINT('Ctrl Pts',(48.7830207157406,-63.8810596700917,-455.541370214754));
#33279=CARTESIAN_POINT('Ctrl Pts',(48.782863222178,-63.8809232969282,-455.541585134083));
#33280=CARTESIAN_POINT('Ctrl Pts',(56.8163034073806,-75.4539484719562,-440.982509561286));
#33281=CARTESIAN_POINT('Ctrl Pts',(56.8017229870639,-75.4445663251619,-441.000077552423));
#33282=CARTESIAN_POINT('Ctrl Pts',(44.7374479017925,-67.6814979527012,-455.536357931381));
#33283=CARTESIAN_POINT('Ctrl Pts',(44.7372694651336,-67.6813831330396,-455.536572930234));
#33284=CARTESIAN_POINT('Ctrl Pts',(56.8145878317028,-75.4554682469289,-440.982509624012));
#33285=CARTESIAN_POINT('Ctrl Pts',(56.800006309516,-75.4460872569967,-441.000077602904));
#33286=CARTESIAN_POINT('Ctrl Pts',(44.734812610957,-67.6839735626181,-455.536354666374));
#33287=CARTESIAN_POINT('Ctrl Pts',(44.7346341606556,-67.6838587569965,-455.536569665279));
#33288=CARTESIAN_POINT('Ctrl Pts',(56.8128722560251,-75.4569880219015,-440.982509686737));
#33289=CARTESIAN_POINT('Ctrl Pts',(56.798289631968,-75.4476081888316,-441.000077653386));
#33290=CARTESIAN_POINT('Ctrl Pts',(44.7321773201212,-67.686449172535,-455.536351401367));
#33291=CARTESIAN_POINT('Ctrl Pts',(44.7319988561776,-67.6863343809532,-455.536566400323));
#33292=CARTESIAN_POINT('Ctrl Pts',(56.8111566803473,-75.4585077968741,-440.982509749462));
#33293=CARTESIAN_POINT('Ctrl Pts',(56.7965729544201,-75.4491291206665,-441.000077703867));
#33294=CARTESIAN_POINT('Ctrl Pts',(44.7295420292855,-67.6889247824519,-455.536348136359));
#33295=CARTESIAN_POINT('Ctrl Pts',(44.7293635516996,-67.6888100049102,-455.536563135368));
#33296=CARTESIAN_POINT('Ctrl Pts',(56.8017229870589,-75.4445663251663,-441.000077552423));
#33297=CARTESIAN_POINT('Ctrl Pts',(56.8648198811864,-75.3888096554507,-440.999961040072));
#33298=CARTESIAN_POINT('Ctrl Pts',(56.9490629520645,-75.3142041475122,-440.99980826392));
#33299=CARTESIAN_POINT('Ctrl Pts',(57.1309026962115,-75.1522669958779,-440.999493603969));
#33300=CARTESIAN_POINT('Ctrl Pts',(57.2129563206459,-75.0789104508246,-440.999356367237));
#33301=CARTESIAN_POINT('Ctrl Pts',(57.4587061305076,-74.8583554202793,-440.998959410034));
#33302=CARTESIAN_POINT('Ctrl Pts',(57.6219769384721,-74.7106841995689,-440.998714462169));
#33303=CARTESIAN_POINT('Ctrl Pts',(58.1101297576784,-74.2657415537038,-440.998037197435));
#33304=CARTESIAN_POINT('Ctrl Pts',(58.4332925903842,-73.9665939710789,-440.997662466009));
#33305=CARTESIAN_POINT('Ctrl Pts',(59.3960169304096,-73.0615413671499,-440.996760635968));
#33306=CARTESIAN_POINT('Ctrl Pts',(60.0285620594009,-72.4482523252744,-440.996454799799));
#33307=CARTESIAN_POINT('Ctrl Pts',(61.2742044918225,-71.2027168180214,-440.996429126657));
#33308=CARTESIAN_POINT('Ctrl Pts',(61.8872423624114,-70.5705492064193,-440.996708949208));
#33309=CARTESIAN_POINT('Ctrl Pts',(62.7920842157113,-69.6082439366836,-440.997600483858));
#33310=CARTESIAN_POINT('Ctrl Pts',(63.091261927389,-69.2851139850578,-440.997976729447));
#33311=CARTESIAN_POINT('Ctrl Pts',(63.536287614412,-68.7969688084124,-440.998667403033));
#33312=CARTESIAN_POINT('Ctrl Pts',(63.6840113457327,-68.6336726425307,-440.998918717446));
#33313=CARTESIAN_POINT('Ctrl Pts',(63.9046541692162,-68.3878737184406,-440.999328524882));
#33314=CARTESIAN_POINT('Ctrl Pts',(63.9780461765651,-68.3057965653884,-440.999470605172));
#33315=CARTESIAN_POINT('Ctrl Pts',(64.1400134581583,-68.1239584591725,-440.999797190977));
#33316=CARTESIAN_POINT('Ctrl Pts',(64.2146497815168,-68.0396973166364,-440.999956381979));
#33317=CARTESIAN_POINT('Ctrl Pts',(64.2705054959405,-67.9765004273713,-441.000078147039));
#33318=CARTESIAN_POINT('Ctrl Pts',(56.5915605594697,-42.9638796623104,-462.499999999983));
#33319=CARTESIAN_POINT('Ctrl Pts',(56.5747906715002,-42.9493768901674,-462.527334954314));
#33320=CARTESIAN_POINT('Ctrl Pts',(56.0041009291271,-45.6723857139866,-462.499999999983));
#33321=CARTESIAN_POINT('Ctrl Pts',(55.9871198863777,-45.6551025508765,-462.52696699751));
#33322=CARTESIAN_POINT('Ctrl Pts',(54.7064708585618,-48.1213181444985,-462.499999999982));
#33323=CARTESIAN_POINT('Ctrl Pts',(54.6902576362458,-48.1011934320598,-462.52696699751));
#33324=CARTESIAN_POINT('Ctrl Pts',(52.7925979348378,-50.1295710081989,-462.498943458986));
#33325=CARTESIAN_POINT('Ctrl Pts',(52.7780049328352,-50.1068804371721,-462.52627709823));
#33326=CARTESIAN_POINT('Origin',(54.2736315587506,-11.1690000000061,-438.999999999986));
#33327=CARTESIAN_POINT('Ctrl Pts',(70.512394258107,12.4256934496976,-438.999999999989));
#33328=CARTESIAN_POINT('Ctrl Pts',(70.4806962609452,12.7626097179399,-438.999999999989));
#33329=CARTESIAN_POINT('Ctrl Pts',(70.4604150062139,13.1004968020805,-438.999999999987));
#33330=CARTESIAN_POINT('Ctrl Pts',(70.4427152853469,13.7773550845288,-438.999999999987));
#33331=CARTESIAN_POINT('Ctrl Pts',(70.4453211759903,14.1161237170503,-438.99999999999));
#33332=CARTESIAN_POINT('Ctrl Pts',(70.4593636589103,14.4545180952481,-438.99999999999));
#33333=CARTESIAN_POINT('Ctrl Pts',(69.7886736272828,32.0388792074281,-440.988676628513));
#33334=CARTESIAN_POINT('Ctrl Pts',(69.7816652336223,32.0328182762799,-441.000100325617));
#33335=CARTESIAN_POINT('Ctrl Pts',(56.5915605594642,20.6258796622937,-462.49999999999));
#33336=CARTESIAN_POINT('Ctrl Pts',(56.5783704547901,20.6144727236797,-462.521499899664));
#33337=CARTESIAN_POINT('Ctrl Pts',(69.9838203851238,27.6573003811947,-440.988601378206));
#33338=CARTESIAN_POINT('Ctrl Pts',(69.9770872889492,27.6518995318566,-440.999999999991));
#33339=CARTESIAN_POINT('Ctrl Pts',(57.2771687825099,17.4648556101157,-462.499999999989));
#33340=CARTESIAN_POINT('Ctrl Pts',(57.2644408666264,17.4546461085292,-462.521547397428));
#33341=CARTESIAN_POINT('Ctrl Pts',(70.1541602115504,23.274511221385,-440.988622685345));
#33342=CARTESIAN_POINT('Ctrl Pts',(70.1476583281893,23.2697541556268,-440.99999999999));
#33343=CARTESIAN_POINT('Ctrl Pts',(57.8608844602741,14.2802063587041,-462.49999999999));
#33344=CARTESIAN_POINT('Ctrl Pts',(57.8485475387408,14.2711801206548,-462.521587750835));
#33345=CARTESIAN_POINT('Ctrl Pts',(70.2996831943332,18.890636417085,-440.988740602151));
#33346=CARTESIAN_POINT('Ctrl Pts',(70.2933682482186,18.8865091831852,-441.000100380184));
#33347=CARTESIAN_POINT('Ctrl Pts',(58.3414879230458,11.0751668932784,-462.499999999988));
#33348=CARTESIAN_POINT('Ctrl Pts',(58.3294687920448,11.0673115982351,-462.521620874947));
#33349=CARTESIAN_POINT('Ctrl Pts',(70.2997304533948,18.8892127394985,-440.988740640445));
#33350=CARTESIAN_POINT('Ctrl Pts',(70.2934155679886,18.8850857101388,-441.000100412783));
#33351=CARTESIAN_POINT('Ctrl Pts',(58.3416442407962,11.0741244443621,-462.499999999988));
#33352=CARTESIAN_POINT('Ctrl Pts',(58.3296252131575,11.0662695301716,-462.521620885722));
#33353=CARTESIAN_POINT('Ctrl Pts',(70.2997777124563,18.887789061912,-440.988740678739));
#33354=CARTESIAN_POINT('Ctrl Pts',(70.2934628877585,18.8836622370922,-441.000100445382));
#33355=CARTESIAN_POINT('Ctrl Pts',(58.3418005585465,11.0730819954458,-462.499999999988));
#33356=CARTESIAN_POINT('Ctrl Pts',(58.32978163427,11.0652274621081,-462.521620896496));
#33357=CARTESIAN_POINT('Ctrl Pts',(70.2998249715178,18.8863653843256,-440.988740717032));
#33358=CARTESIAN_POINT('Ctrl Pts',(70.2935102075285,18.8822387640455,-441.00010047798));
#33359=CARTESIAN_POINT('Ctrl Pts',(58.3419568762969,11.0720395465295,-462.499999999988));
#33360=CARTESIAN_POINT('Ctrl Pts',(58.3299380553828,11.0641853940446,-462.521620907269));
#33361=CARTESIAN_POINT('Ctrl Pts',(70.2929704412094,18.89898172966,-441.000070381186));
#33362=CARTESIAN_POINT('Ctrl Pts',(69.4478798152777,18.703333595985,-442.499259503123));
#33363=CARTESIAN_POINT('Ctrl Pts',(68.5970566354322,18.4935685970824,-443.998044926457));
#33364=CARTESIAN_POINT('Ctrl Pts',(66.921371690547,18.0525189012106,-446.927744712079));
#33365=CARTESIAN_POINT('Ctrl Pts',(66.0883452949664,17.8200628885466,-448.373677904118));
#33366=CARTESIAN_POINT('Ctrl Pts',(65.2503505017821,17.5706789545087,-449.81715836622));
#33367=CARTESIAN_POINT('Ctrl Pts',(64.5871672591961,17.3700458363661,-450.95723971308));
#33368=CARTESIAN_POINT('Ctrl Pts',(63.402389223456,17.0056913908832,-452.989932143487));
#33369=CARTESIAN_POINT('Ctrl Pts',(62.210822170982,16.6072491489963,-455.011995086995));
#33370=CARTESIAN_POINT('Ctrl Pts',(59.9333797132287,15.7661053116544,-458.839522722581));
#33371=CARTESIAN_POINT('Ctrl Pts',(58.8249846736614,15.3210207890733,-460.685225965698));
#33372=CARTESIAN_POINT('Ctrl Pts',(57.7295804999066,14.8304431732807,-462.499999999989));
#33373=CARTESIAN_POINT('Ctrl Pts',(70.2996831378601,-41.2286363801844,-440.988740703741));
#33374=CARTESIAN_POINT('Ctrl Pts',(70.2933682482237,-41.2245091831969,-441.000100380177));
#33375=CARTESIAN_POINT('Ctrl Pts',(58.3414879230496,-33.4131668932962,-462.499999999984));
#33376=CARTESIAN_POINT('Ctrl Pts',(58.3294687920485,-33.4053115982529,-462.521620874943));
#33377=CARTESIAN_POINT('Ctrl Pts',(70.1541601534062,-45.6125111788507,-440.988622787091));
#33378=CARTESIAN_POINT('Ctrl Pts',(70.1476583281953,-45.607754155638,-440.999999999982));
#33379=CARTESIAN_POINT('Ctrl Pts',(57.8608844602783,-36.6182063587215,-462.499999999984));
#33380=CARTESIAN_POINT('Ctrl Pts',(57.8485475387452,-36.6091801206722,-462.521587750829));
#33381=CARTESIAN_POINT('Ctrl Pts',(69.9838203249125,-49.9953003329024,-440.988601480142));
#33382=CARTESIAN_POINT('Ctrl Pts',(69.977087288956,-49.9898995318672,-440.999999999982));
#33383=CARTESIAN_POINT('Ctrl Pts',(57.2771687825149,-39.8028556101327,-462.499999999983));
#33384=CARTESIAN_POINT('Ctrl Pts',(57.2644408666313,-39.7926461085464,-462.521547397421));
#33385=CARTESIAN_POINT('Ctrl Pts',(69.7886735646101,-54.3768791532312,-440.988676730672));
#33386=CARTESIAN_POINT('Ctrl Pts',(69.7816652336298,-54.3708182762895,-441.000100325607));
#33387=CARTESIAN_POINT('Ctrl Pts',(56.5915605594697,-42.9638796623104,-462.499999999983));
#33388=CARTESIAN_POINT('Ctrl Pts',(56.5783704547956,-42.9524727236964,-462.521499899657));
#33389=CARTESIAN_POINT('Origin',(22.4991425263181,166.837401348805,-389.327908649814));
#33390=CARTESIAN_POINT('Origin',(54.2736315587506,-11.1690000000061,-438.999999999986));
#33391=CARTESIAN_POINT('Ctrl Pts',(57.867944997635,-37.6757543779957,-462.508620368993));
#33392=CARTESIAN_POINT('Ctrl Pts',(57.872959299689,-37.6772709866423,-462.499999999983));
#33393=CARTESIAN_POINT('Ctrl Pts',(71.5424551348726,-41.8116999372577,-438.999999999983));
#33394=CARTESIAN_POINT('Ctrl Pts',(71.5463747327639,-41.8128854454279,-438.993261598541));
#33395=CARTESIAN_POINT('Ctrl Pts',(57.8719099587016,-37.6887260106591,-462.508620581582));
#33396=CARTESIAN_POINT('Ctrl Pts',(57.8769250855219,-37.6902432536445,-462.499999999983));
#33397=CARTESIAN_POINT('Ctrl Pts',(71.5483174526145,-41.8262325427425,-438.999989167174));
#33398=CARTESIAN_POINT('Ctrl Pts',(71.5522375084354,-41.8274184918791,-438.993250925682));
#33399=CARTESIAN_POINT('Ctrl Pts',(57.8758749197681,-37.7016976433226,-462.508620794173));
#33400=CARTESIAN_POINT('Ctrl Pts',(57.8808908713546,-37.7032155206467,-462.499999999983));
#33401=CARTESIAN_POINT('Ctrl Pts',(71.5541797703564,-41.8407651482274,-438.999978334365));
#33402=CARTESIAN_POINT('Ctrl Pts',(71.5581002841068,-41.8419515383303,-438.993240252822));
#33403=CARTESIAN_POINT('Ctrl Pts',(57.8798398808347,-37.7146692759861,-462.508621006763));
#33404=CARTESIAN_POINT('Ctrl Pts',(57.8848566571874,-37.7161877876489,-462.499999999983));
#33405=CARTESIAN_POINT('Ctrl Pts',(71.5600420880984,-41.8552977537122,-438.999967501557));
#33406=CARTESIAN_POINT('Ctrl Pts',(71.5639630597783,-41.8564845847815,-438.993229579963));
#33407=CARTESIAN_POINT('Ctrl Pts',(59.0902650976022,-21.634493046715,-462.499999999985));
#33408=CARTESIAN_POINT('Ctrl Pts',(70.7709995585468,-23.4880802833718,-439.80032773308));
#33409=CARTESIAN_POINT('Ctrl Pts',(59.6440060900487,-24.2785347615132,-462.499999999984));
#33410=CARTESIAN_POINT('Ctrl Pts',(71.4248025866704,-26.3361222680391,-439.789824991753));
#33411=CARTESIAN_POINT('Ctrl Pts',(59.3774521833123,-26.966756235111,-462.499999999984));
#33412=CARTESIAN_POINT('Ctrl Pts',(71.353329194899,-29.2564718771875,-439.789824991753));
#33413=CARTESIAN_POINT('Ctrl Pts',(58.315252633502,-29.4505673778293,-462.499999999984));
#33414=CARTESIAN_POINT('Ctrl Pts',(70.5621815020438,-32.0667859302444,-439.798062313332));
#33415=CARTESIAN_POINT('',(59.0902650976022,-21.6344930467149,-462.499999999985));
#33416=CARTESIAN_POINT('Origin',(54.2736315587506,-11.1690000000061,-438.999999999986));
#33417=CARTESIAN_POINT('Ctrl Pts',(70.7611151580493,-20.5658120600565,-438.999999999985));
#33418=CARTESIAN_POINT('Ctrl Pts',(70.7414378019089,-20.2008497257058,-438.999999999986));
#33419=CARTESIAN_POINT('Ctrl Pts',(70.7332146113695,-19.8353710262216,-438.999999999986));
#33420=CARTESIAN_POINT('Ctrl Pts',(70.7396988669432,-19.1051660456595,-438.999999999986));
#33421=CARTESIAN_POINT('Ctrl Pts',(70.754357444811,-18.7406409415397,-438.999999999986));
#33422=CARTESIAN_POINT('Ctrl Pts',(70.7804124467093,-18.3768313194476,-438.999999999986));
#33423=CARTESIAN_POINT('Ctrl Pts',(59.4064050032676,-15.0625633529524,-462.499999999986));
#33424=CARTESIAN_POINT('Ctrl Pts',(71.2535130610729,-15.3970838267174,-439.002429127845));
#33425=CARTESIAN_POINT('Ctrl Pts',(58.7385280596113,-17.2020528032917,-462.499999999986));
#33426=CARTESIAN_POINT('Ctrl Pts',(70.5853951815301,-18.0862311145172,-438.998932713963));
#33427=CARTESIAN_POINT('Ctrl Pts',(58.6308352736733,-19.4407749798555,-462.499999999985));
#33428=CARTESIAN_POINT('Ctrl Pts',(70.5610300866927,-20.8529288319753,-438.998910332345));
#33429=CARTESIAN_POINT('Ctrl Pts',(59.0902650976022,-21.634493046715,-462.499999999985));
#33430=CARTESIAN_POINT('Ctrl Pts',(71.1815697946312,-23.5532326718541,-439.002448983861));
#33431=CARTESIAN_POINT('',(59.4064050032676,-15.0625633529524,-462.499999999986));
#33432=CARTESIAN_POINT('Ctrl Pts',(59.406405003267,-7.27543664706474,-462.499999999987));
#33433=CARTESIAN_POINT('Ctrl Pts',(70.7822037837443,-6.95422428207083,-439.937224614869));
#33434=CARTESIAN_POINT('Ctrl Pts',(60.204044757483,-9.83061070349041,-462.499999999987));
#33435=CARTESIAN_POINT('Ctrl Pts',(71.4803706009395,-9.73514197376118,-439.927462314949));
#33436=CARTESIAN_POINT('Ctrl Pts',(60.2040447574833,-12.5073892965266,-462.499999999986));
#33437=CARTESIAN_POINT('Ctrl Pts',(71.4803706009397,-12.602858026249,-439.927462314949));
#33438=CARTESIAN_POINT('Ctrl Pts',(59.4064050032676,-15.0625633529524,-462.499999999986));
#33439=CARTESIAN_POINT('Ctrl Pts',(70.782203783745,-15.3837757179391,-439.937224614867));
#33440=CARTESIAN_POINT('',(59.406405003267,-7.27543664706474,-462.499999999987));
#33441=CARTESIAN_POINT('Origin',(54.2736315587506,-11.1690000000061,-438.999999999986));
#33442=CARTESIAN_POINT('Ctrl Pts',(70.7804124467082,-3.96116868056056,-438.999999999988));
#33443=CARTESIAN_POINT('Ctrl Pts',(70.7543859912015,-3.59775765571275,-438.999999999988));
#33444=CARTESIAN_POINT('Ctrl Pts',(70.7397309932481,-3.23363260618974,-438.999999999988));
#33445=CARTESIAN_POINT('Ctrl Pts',(70.7331966490285,-2.50342807144109,-438.999999999988));
#33446=CARTESIAN_POINT('Ctrl Pts',(70.7414162872563,-2.1375493135523,-438.999999999987));
#33447=CARTESIAN_POINT('Ctrl Pts',(70.7611151580477,-1.77218793995684,-438.999999999987));
#33448=CARTESIAN_POINT('Ctrl Pts',(59.0902650976006,-0.703506953302192,
-462.499999999988));
#33449=CARTESIAN_POINT('Ctrl Pts',(71.1815697946293,1.21523267184444,-439.002448983864));
#33450=CARTESIAN_POINT('Ctrl Pts',(58.630835273672,-2.8972250201618,-462.499999999987));
#33451=CARTESIAN_POINT('Ctrl Pts',(70.5610300866923,-1.48507116802909,-438.998910332348));
#33452=CARTESIAN_POINT('Ctrl Pts',(58.7385280596104,-5.13594719672545,-462.499999999987));
#33453=CARTESIAN_POINT('Ctrl Pts',(70.585395181528,-4.25176888548718,-438.998932713964));
#33454=CARTESIAN_POINT('Ctrl Pts',(59.406405003267,-7.27543664706474,-462.499999999987));
#33455=CARTESIAN_POINT('Ctrl Pts',(71.2535130610722,-6.94091617329225,-439.002429127846));
#33456=CARTESIAN_POINT('',(59.0902650976006,-0.703506953302192,-462.499999999987));
#33457=CARTESIAN_POINT('Ctrl Pts',(58.3152526334991,7.11256737781201,-462.499999999988));
#33458=CARTESIAN_POINT('Ctrl Pts',(70.5621815020404,9.72878593023445,-439.798062313337));
#33459=CARTESIAN_POINT('Ctrl Pts',(59.3774521833097,4.6287562350939,-462.499999999988));
#33460=CARTESIAN_POINT('Ctrl Pts',(71.353329194896,6.91847187717748,-439.789824991758));
#33461=CARTESIAN_POINT('Ctrl Pts',(59.6440060900465,1.94053476149611,-462.499999999987));
#33462=CARTESIAN_POINT('Ctrl Pts',(71.4248025866678,3.99812226802909,-439.789824991758));
#33463=CARTESIAN_POINT('Ctrl Pts',(59.0902650976006,-0.703506953302192,
-462.499999999988));
#33464=CARTESIAN_POINT('Ctrl Pts',(70.7709995585447,1.15008028336193,-439.800327733084));
#33465=CARTESIAN_POINT('',(58.3152526334991,7.11256737781201,-462.499999999988));
#33466=CARTESIAN_POINT('Ctrl Pts',(57.8729592854362,15.3392709400169,-462.499999999989));
#33467=CARTESIAN_POINT('Ctrl Pts',(71.5424551136857,19.4736998850754,-438.99999999999));
#33468=CARTESIAN_POINT('Ctrl Pts',(57.002852784826,12.4931127039992,-462.499999999989));
#33469=CARTESIAN_POINT('Ctrl Pts',(70.2493774538459,16.2681780209163,-439.002389441071));
#33470=CARTESIAN_POINT('Ctrl Pts',(57.2363227433815,9.63550017679799,-462.499999999989));
#33471=CARTESIAN_POINT('Ctrl Pts',(70.1312984442438,12.9284311565945,-438.996844362213));
#33472=CARTESIAN_POINT('Ctrl Pts',(58.3152526334991,7.11256737781201,-462.499999999988));
#33473=CARTESIAN_POINT('Ctrl Pts',(70.9913620171455,9.8204685094352,-439.002497203518));
#33474=CARTESIAN_POINT('Ctrl Pts',(52.7925979348309,27.7915710081813,-462.498943458995));
#33475=CARTESIAN_POINT('Ctrl Pts',(52.7792868797399,27.7708737286954,-462.523875928528));
#33476=CARTESIAN_POINT('Ctrl Pts',(54.7064708585553,25.7833181444813,-462.499999999991));
#33477=CARTESIAN_POINT('Ctrl Pts',(54.6916819141412,25.7649613214017,-462.524598036068));
#33478=CARTESIAN_POINT('Ctrl Pts',(56.0041009291211,23.3343857139696,-462.49999999999));
#33479=CARTESIAN_POINT('Ctrl Pts',(55.9886116147567,23.318620819518,-462.524598036068));
#33480=CARTESIAN_POINT('Ctrl Pts',(56.5915605594642,20.6258796622937,-462.49999999999));
#33481=CARTESIAN_POINT('Ctrl Pts',(56.5762638506312,20.6126509106678,-462.524933669083));
#33482=CARTESIAN_POINT('Ctrl Pts',(56.6115466725153,53.2965039304289,-440.982369050107));
#33483=CARTESIAN_POINT('Ctrl Pts',(56.597010807163,53.2869057865868,-441.00007767524));
#33484=CARTESIAN_POINT('Ctrl Pts',(56.6133279334121,53.2949358941234,-440.982368985934));
#33485=CARTESIAN_POINT('Ctrl Pts',(56.5987931490312,53.2853365991255,-441.000077624278));
#33486=CARTESIAN_POINT('Ctrl Pts',(56.6151091943089,53.2933678578181,-440.982368921762));
#33487=CARTESIAN_POINT('Ctrl Pts',(56.6005754908994,53.2837674116641,-441.000077573315));
#33488=CARTESIAN_POINT('Ctrl Pts',(56.6168904552057,53.2917998215128,-440.98236885759));
#33489=CARTESIAN_POINT('Ctrl Pts',(56.6023578327675,53.2821982242028,-441.000077522351));
#33490=CARTESIAN_POINT('Ctrl Pts',(59.3264760633801,50.9065632659512,-440.982271241517));
#33491=CARTESIAN_POINT('Ctrl Pts',(59.3135877730366,50.8952105744222,-440.999999999993));
#33492=CARTESIAN_POINT('Ctrl Pts',(61.8829281942602,48.3583918787876,-440.982271241516));
#33493=CARTESIAN_POINT('Ctrl Pts',(61.8717342174682,48.3453380510862,-440.999999999993));
#33494=CARTESIAN_POINT('Ctrl Pts',(64.2799598697074,45.6532009762712,-440.982369491764));
#33495=CARTESIAN_POINT('Ctrl Pts',(64.2705054959308,45.6385004273605,-441.000078147052));
#33496=CARTESIAN_POINT('Ctrl Pts',(64.2815357486139,45.6514225044533,-440.982369556356));
#33497=CARTESIAN_POINT('Ctrl Pts',(64.2720825185032,45.6367208729398,-441.000078198428));
#33498=CARTESIAN_POINT('Ctrl Pts',(64.2831116275205,45.6496440326354,-440.982369620949));
#33499=CARTESIAN_POINT('Ctrl Pts',(64.2736595410759,45.6349413185191,-441.000078249804));
#33500=CARTESIAN_POINT('Ctrl Pts',(64.2846875064269,45.6478655608175,-440.982369685541));
#33501=CARTESIAN_POINT('Ctrl Pts',(64.2752365636483,45.6331617640984,-441.000078301181));
#33502=CARTESIAN_POINT('Ctrl Pts',(64.2705054959311,45.6385004273602,-441.000078147052));
#33503=CARTESIAN_POINT('Ctrl Pts',(64.2132896438939,45.7032361413531,-440.999956345651));
#33504=CARTESIAN_POINT('Ctrl Pts',(64.1367868626771,45.789599828806,-440.999797014702));
#33505=CARTESIAN_POINT('Ctrl Pts',(63.9707562357255,45.9759636633542,-440.999470182454));
#33506=CARTESIAN_POINT('Ctrl Pts',(63.8955272911772,46.0600707364969,-440.99932802141));
#33507=CARTESIAN_POINT('Ctrl Pts',(63.6693479463854,46.3119401271007,-440.998918002061));
#33508=CARTESIAN_POINT('Ctrl Pts',(63.5179009198511,46.4792552858216,-440.998666591105));
#33509=CARTESIAN_POINT('Ctrl Pts',(63.061604480683,46.9793778842359,-440.9979756921));
#33510=CARTESIAN_POINT('Ctrl Pts',(62.7547855853059,47.3103786533786,-440.997599393785));
#33511=CARTESIAN_POINT('Ctrl Pts',(61.8266329871262,48.2959593976243,-440.99670763129));
#33512=CARTESIAN_POINT('Ctrl Pts',(61.1975600856359,48.9431704863275,-440.996427551129));
#33513=CARTESIAN_POINT('Ctrl Pts',(59.9186211802959,50.218080636068,-440.996452059618));
#33514=CARTESIAN_POINT('Ctrl Pts',(59.2688114468007,50.8456859164495,-440.996757235888));
#33515=CARTESIAN_POINT('Ctrl Pts',(58.2795110232487,51.7714152778138,-440.997659002473));
#33516=CARTESIAN_POINT('Ctrl Pts',(57.9473806255298,52.0773186454005,-440.99803387866));
#33517=CARTESIAN_POINT('Ctrl Pts',(57.4456133245308,52.5321901467099,-440.998711889762));
#33518=CARTESIAN_POINT('Ctrl Pts',(57.2777787398507,52.6831355444427,-440.998957173669));
#33519=CARTESIAN_POINT('Ctrl Pts',(57.0251433367402,52.9085499906903,-440.999354813187));
#33520=CARTESIAN_POINT('Ctrl Pts',(56.9407883129355,52.9835173208311,-440.9994923065));
#33521=CARTESIAN_POINT('Ctrl Pts',(56.8140360711639,53.0957164489069,-440.999706086766));
#33522=CARTESIAN_POINT('Ctrl Pts',(56.7717497004109,53.1330733071561,-440.999778601897));
#33523=CARTESIAN_POINT('Ctrl Pts',(56.6780978857083,53.2156432553775,-440.999941865624));
#33524=CARTESIAN_POINT('Ctrl Pts',(56.6347709042445,53.2537341362971,-441.00001916926));
#33525=CARTESIAN_POINT('Ctrl Pts',(56.6023578328018,53.2821982241729,-441.000077522351));
#33526=CARTESIAN_POINT('Ctrl Pts',(41.9546679377988,60.6647702916318,-440.977450556666));
#33527=CARTESIAN_POINT('Ctrl Pts',(41.9445347128706,60.6495679335285,-440.998916834174));
#33528=CARTESIAN_POINT('Ctrl Pts',(47.4212267268272,59.4923192195593,-440.97860778164));
#33529=CARTESIAN_POINT('Ctrl Pts',(47.4083864201783,59.4777499755747,-440.999999999994));
#33530=CARTESIAN_POINT('Ctrl Pts',(52.4160636430517,56.9796669347799,-440.97860778164));
#33531=CARTESIAN_POINT('Ctrl Pts',(52.4006927127278,56.9663054203067,-440.999999999994));
#33532=CARTESIAN_POINT('Ctrl Pts',(56.6199725617386,53.2938361467473,-440.978613169889));
#33533=CARTESIAN_POINT('Ctrl Pts',(56.6023578327675,53.2821982242028,-441.000077522351));
#33534=CARTESIAN_POINT('Ctrl Pts',(56.6023578327673,53.2821982242029,-441.000077522352));
#33535=CARTESIAN_POINT('Ctrl Pts',(54.630099851199,55.0143046797825,-440.997830128999));
#33536=CARTESIAN_POINT('Ctrl Pts',(52.4556758675906,56.5016643215144,-440.996476847209));
#33537=CARTESIAN_POINT('Ctrl Pts',(47.6685347341379,58.9889857335417,-440.994366068387));
#33538=CARTESIAN_POINT('Ctrl Pts',(45.0577394529488,59.947352817005,-440.993641905209));
#33539=CARTESIAN_POINT('Ctrl Pts',(42.2210187024469,60.5949101226765,-440.992100692275));
#33540=CARTESIAN_POINT('Ctrl Pts',(42.08451707017,60.6251470261161,-440.992024703487));
#33541=CARTESIAN_POINT('Ctrl Pts',(41.9478250221979,60.654504216007,-440.991946625419));
#33542=CARTESIAN_POINT('Origin',(0.583570446910677,-20.4591843142083,-487.927777712865));
#33543=CARTESIAN_POINT('',(33.4816044331148,62.276074524876,-440.9999972802));
#33544=CARTESIAN_POINT('Ctrl Pts',(18.8780323328947,47.6381153531325,-462.499937569615));
#33545=CARTESIAN_POINT('Ctrl Pts',(20.9284013294519,49.6296583969895,-459.596795658369));
#33546=CARTESIAN_POINT('Ctrl Pts',(22.9543862194209,51.628750133794,-456.668452986475));
#33547=CARTESIAN_POINT('Ctrl Pts',(27.8203525467718,56.4898863340891,-449.530713795769));
#33548=CARTESIAN_POINT('Ctrl Pts',(30.6950354236204,59.4116076064736,-445.226004279766));
#33549=CARTESIAN_POINT('Ctrl Pts',(33.4816127180597,62.2760728748087,-441.00000162475));
#33550=CARTESIAN_POINT('Ctrl Pts',(41.9449609251821,60.6486156188608,-441.000894783878));
#33551=CARTESIAN_POINT('Ctrl Pts',(39.1229463094741,61.2547168564534,-440.998260847152));
#33552=CARTESIAN_POINT('Ctrl Pts',(36.3000689160198,61.7969223748677,-440.998848881191));
#33553=CARTESIAN_POINT('Ctrl Pts',(33.4816044833662,62.2760748116437,-441.000000948612));
#33554=CARTESIAN_POINT('Origin',(29.9999999999753,83.0468894509273,-439.));
#33555=CARTESIAN_POINT('',(28.3882740955986,63.1097913591115,-438.999999999994));
#33556=CARTESIAN_POINT('',(26.1596537758254,63.4168994820682,-438.999999999994));
#33557=CARTESIAN_POINT('Origin',(-0.00176539235111073,-134.670997806539,
-438.999999999971));
#33558=CARTESIAN_POINT('Ctrl Pts',(28.3882740955984,63.1097913591091,-438.999999999998));
#33559=CARTESIAN_POINT('Ctrl Pts',(28.0150890543069,63.1396553617187,-438.999999999998));
#33560=CARTESIAN_POINT('Ctrl Pts',(27.6425418332694,63.1800897025264,-438.999999999998));
#33561=CARTESIAN_POINT('Ctrl Pts',(26.8985866816018,63.2826197832723,-438.999999999998));
#33562=CARTESIAN_POINT('Ctrl Pts',(26.528147392113,63.3445453679781,-438.999999999998));
#33563=CARTESIAN_POINT('Ctrl Pts',(26.1596537758248,63.4168994820655,-438.999999999998));
#33564=CARTESIAN_POINT('Ctrl Pts',(12.0088324072726,47.904965729667,-462.504463162543));
#33565=CARTESIAN_POINT('Ctrl Pts',(12.0109810190255,47.9080583287232,-462.499999999992));
#33566=CARTESIAN_POINT('Ctrl Pts',(23.3245997914203,64.1922877582739,-438.999002412958));
#33567=CARTESIAN_POINT('Ctrl Pts',(23.3284217331517,64.1977888607304,-438.991063357806));
#33568=CARTESIAN_POINT('Ctrl Pts',(12.0101894276276,47.9043018479569,-462.50446316207));
#33569=CARTESIAN_POINT('Ctrl Pts',(12.0123383942081,47.9073943572616,-462.499999999992));
#33570=CARTESIAN_POINT('Ctrl Pts',(23.3278255288872,64.1911511953027,-438.999004902713));
#33571=CARTESIAN_POINT('Ctrl Pts',(23.3316481017846,64.1966521381094,-438.991065848401));
#33572=CARTESIAN_POINT('Ctrl Pts',(12.0115464479826,47.9036379662469,-462.504463161597));
#33573=CARTESIAN_POINT('Ctrl Pts',(12.0136957693908,47.9067303858,-462.499999999992));
#33574=CARTESIAN_POINT('Ctrl Pts',(23.3310512663538,64.1900146323315,-438.999007392467));
#33575=CARTESIAN_POINT('Ctrl Pts',(23.3348744704173,64.1955154154884,-438.991068338997));
#33576=CARTESIAN_POINT('Ctrl Pts',(12.0129034683376,47.9029740845369,-462.504463161124));
#33577=CARTESIAN_POINT('Ctrl Pts',(12.0150531445734,47.9060664143383,-462.499999999992));
#33578=CARTESIAN_POINT('Ctrl Pts',(23.3342770038207,64.1888780693604,-438.999009882221));
#33579=CARTESIAN_POINT('Ctrl Pts',(23.3381008390501,64.1943786928674,-438.991070829592));
#33580=CARTESIAN_POINT('Ctrl Pts',(12.5525590984298,47.6389636728949,-462.504462973087));
#33581=CARTESIAN_POINT('Ctrl Pts',(12.554849881435,47.6420203105494,-462.499999999992));
#33582=CARTESIAN_POINT('Ctrl Pts',(24.6170782372489,63.7368932453292,-438.999999999994));
#33583=CARTESIAN_POINT('Ctrl Pts',(24.621153072618,63.7423303797924,-438.992061281844));
#33584=CARTESIAN_POINT('Ctrl Pts',(13.1531317256866,47.4164397049396,-462.504462963041));
#33585=CARTESIAN_POINT('Ctrl Pts',(13.1555740488351,47.4194722561805,-462.499999999992));
#33586=CARTESIAN_POINT('Ctrl Pts',(26.0157443355876,63.3875170188384,-439.000052901838));
#33587=CARTESIAN_POINT('Ctrl Pts',(26.0200887299393,63.3929113084884,-438.992114201559));
#33588=CARTESIAN_POINT('Ctrl Pts',(14.4571112437118,47.110317095545,-462.504462977168));
#33589=CARTESIAN_POINT('Ctrl Pts',(14.4598710640546,47.1133367987093,-462.499999999992));
#33590=CARTESIAN_POINT('Ctrl Pts',(28.9918381339846,63.0137293945006,-438.999978514899));
#33591=CARTESIAN_POINT('Ctrl Pts',(28.996747291037,63.0191008300449,-438.992039789491));
#33592=CARTESIAN_POINT('Ctrl Pts',(15.1606676247628,47.0274060982099,-462.504462973087));
#33593=CARTESIAN_POINT('Ctrl Pts',(15.1635931228085,47.0304369741072,-462.499999999992));
#33594=CARTESIAN_POINT('Ctrl Pts',(30.567944125466,62.9896601345561,-438.999999999994));
#33595=CARTESIAN_POINT('Ctrl Pts',(30.5731479893337,62.9950514441119,-438.992061281845));
#33596=CARTESIAN_POINT('Ctrl Pts',(16.619483413463,47.0519242799615,-462.504462973087));
#33597=CARTESIAN_POINT('Ctrl Pts',(16.622742373222,47.0550172977492,-462.499999999992));
#33598=CARTESIAN_POINT('Ctrl Pts',(33.7829521032227,63.3414515780021,-438.999999999994));
#33599=CARTESIAN_POINT('Ctrl Pts',(33.7887491274116,63.3469534252964,-438.992061281845));
#33600=CARTESIAN_POINT('Ctrl Pts',(17.3742915801458,47.1601346920495,-462.504462973087));
#33601=CARTESIAN_POINT('Ctrl Pts',(17.3777182257977,47.1632792121951,-462.499999999992));
#33602=CARTESIAN_POINT('Ctrl Pts',(35.4208861093652,63.7209016414656,-438.999999999994));
#33603=CARTESIAN_POINT('Ctrl Pts',(35.4269814125295,63.726495100942,-438.992061281845));
#33604=CARTESIAN_POINT('Ctrl Pts',(18.3703780276748,47.4490597509409,-462.504462973087));
#33605=CARTESIAN_POINT('Ctrl Pts',(18.374021594636,47.4523013789519,-462.499999999992));
#33606=CARTESIAN_POINT('Ctrl Pts',(37.5593990902821,64.5212499547191,-438.999999999994));
#33607=CARTESIAN_POINT('Ctrl Pts',(37.5658802521772,64.5270161492662,-438.992061281845));
#33608=CARTESIAN_POINT('Ctrl Pts',(18.6243186430052,47.5360060921983,-462.504462973087));
#33609=CARTESIAN_POINT('Ctrl Pts',(18.6280171263085,47.5392751251161,-462.499999999992));
#33610=CARTESIAN_POINT('Ctrl Pts',(38.1025592692013,64.7525255585329,-438.999999999994));
#33611=CARTESIAN_POINT('Ctrl Pts',(38.1091381160596,64.7583405008152,-438.992061281845));
#33612=CARTESIAN_POINT('Ctrl Pts',(18.8747298962646,47.6349689278609,-462.504462973087));
#33613=CARTESIAN_POINT('Ctrl Pts',(18.8784821989614,47.6382677383812,-462.499999999992));
#33614=CARTESIAN_POINT('Ctrl Pts',(38.6364129536412,65.0083135741065,-438.999999999994));
#33615=CARTESIAN_POINT('Ctrl Pts',(38.643087534215,65.0141814846656,-438.992061281845));
#33616=CARTESIAN_POINT('Ctrl Pts',(18.8758942609649,47.6354290862244,-462.504462973087));
#33617=CARTESIAN_POINT('Ctrl Pts',(18.8796468139118,47.6387280352049,-462.499999999992));
#33618=CARTESIAN_POINT('Ctrl Pts',(38.6388952717369,65.009502939729,-438.999999999994));
#33619=CARTESIAN_POINT('Ctrl Pts',(38.6455702974543,65.0153710965805,-438.992061281845));
#33620=CARTESIAN_POINT('Ctrl Pts',(18.8770586256651,47.6358892445878,-462.504462973087));
#33621=CARTESIAN_POINT('Ctrl Pts',(18.8808114288619,47.6391883320286,-462.499999999992));
#33622=CARTESIAN_POINT('Ctrl Pts',(38.6413775898324,65.0106923053514,-438.999999999994));
#33623=CARTESIAN_POINT('Ctrl Pts',(38.6480530606934,65.0165607084954,-438.992061281845));
#33624=CARTESIAN_POINT('Ctrl Pts',(18.8782229903656,47.6363494029513,-462.504462973087));
#33625=CARTESIAN_POINT('Ctrl Pts',(18.8819760438123,47.6396486288522,-462.499999999992));
#33626=CARTESIAN_POINT('Ctrl Pts',(38.643859907928,65.0118816709739,-438.999999999994));
#33627=CARTESIAN_POINT('Ctrl Pts',(38.6505358239326,65.0177503204103,-438.992061281845));
#33628=CARTESIAN_POINT('Ctrl Pts',(33.481598779729,62.2760760009175,-440.999988546436));
#33629=CARTESIAN_POINT('Ctrl Pts',(32.9601399465216,62.3726871929236,-440.550584444613));
#33630=CARTESIAN_POINT('Ctrl Pts',(32.2006722009084,62.5100376689964,-440.020332322067));
#33631=CARTESIAN_POINT('Ctrl Pts',(30.2339613237229,62.8331222144803,-439.276987649111));
#33632=CARTESIAN_POINT('Ctrl Pts',(29.3151615709777,62.9752775583384,-439.083114041147));
#33633=CARTESIAN_POINT('Ctrl Pts',(28.3882740955986,63.1097913591118,-438.999999999994));
#33634=CARTESIAN_POINT('',(23.0582397346304,63.7917958206442,-439.572118888214));
#33635=CARTESIAN_POINT('',(17.5310972153034,55.8409485053149,-451.047580752227));
#33636=CARTESIAN_POINT('Ctrl Pts',(26.1596537758254,63.4168994820685,-438.999999999994));
#33637=CARTESIAN_POINT('Ctrl Pts',(25.6361238202445,63.4852733932441,-439.043651690291));
#33638=CARTESIAN_POINT('Ctrl Pts',(25.113664820537,63.5508806641982,-439.115892043974));
#33639=CARTESIAN_POINT('Ctrl Pts',(23.8409192092728,63.7045947738492,-439.353351910025));
#33640=CARTESIAN_POINT('Ctrl Pts',(23.2599644625544,63.7693502441533,-439.515584934503));
#33641=CARTESIAN_POINT('Ctrl Pts',(23.0582397346378,63.7917958206654,-439.572118888232));
#33642=CARTESIAN_POINT('Ctrl Pts',(7.15508637657014,48.1002682270745,-462.548358098884));
#33643=CARTESIAN_POINT('Ctrl Pts',(7.16823209133649,48.1351541649005,-462.499999999992));
#33644=CARTESIAN_POINT('Ctrl Pts',(13.4012367324298,64.6762260078797,-439.571139897255));
#33645=CARTESIAN_POINT('Ctrl Pts',(13.4078662789118,64.6938194176329,-439.546752310115));
#33646=CARTESIAN_POINT('Ctrl Pts',(7.15842286648213,48.1015224334375,-462.548358080388));
#33647=CARTESIAN_POINT('Ctrl Pts',(7.17157638915753,48.1364081149888,-462.499999999992));
#33648=CARTESIAN_POINT('Ctrl Pts',(13.4082831289197,64.6773584460546,-439.571148667243));
#33649=CARTESIAN_POINT('Ctrl Pts',(13.4149166130267,64.6949517265655,-439.546761089431));
#33650=CARTESIAN_POINT('Ctrl Pts',(7.16175935639413,48.1027766398004,-462.548358061891));
#33651=CARTESIAN_POINT('Ctrl Pts',(7.17492068697853,48.1376620650771,-462.499999999992));
#33652=CARTESIAN_POINT('Ctrl Pts',(13.4153295254096,64.6784908842296,-439.571157437231));
#33653=CARTESIAN_POINT('Ctrl Pts',(13.4219669471417,64.6960840354981,-439.546769868747));
#33654=CARTESIAN_POINT('Ctrl Pts',(7.16509584630612,48.1040308461633,-462.548358043395));
#33655=CARTESIAN_POINT('Ctrl Pts',(7.17826498479954,48.1389160151653,-462.499999999992));
#33656=CARTESIAN_POINT('Ctrl Pts',(13.4223759218995,64.6796233224046,-439.571166207219));
#33657=CARTESIAN_POINT('Ctrl Pts',(13.4290172812566,64.6972163444305,-439.546778648063));
#33658=CARTESIAN_POINT('Ctrl Pts',(7.54205893122661,48.2457335073907,-462.548355953643));
#33659=CARTESIAN_POINT('Ctrl Pts',(7.55611022238567,48.2805897219893,-462.499999999992));
#33660=CARTESIAN_POINT('Ctrl Pts',(14.2184914290542,64.8075683781938,-439.572157057449));
#33661=CARTESIAN_POINT('Ctrl Pts',(14.225577668907,64.8251467981561,-439.547770552181));
#33662=CARTESIAN_POINT('Ctrl Pts',(7.94106123049321,48.3526724298479,-462.548355953643));
#33663=CARTESIAN_POINT('Ctrl Pts',(7.95597858418204,48.3874670903331,-462.499999999992));
#33664=CARTESIAN_POINT('Ctrl Pts',(15.0290009665914,64.8852600322751,-439.572157057449));
#33665=CARTESIAN_POINT('Ctrl Pts',(15.0365239724854,64.902807409737,-439.547770552181));
#33666=CARTESIAN_POINT('Ctrl Pts',(8.76160672396958,48.4833667221507,-462.548355953643));
#33667=CARTESIAN_POINT('Ctrl Pts',(8.77822932150332,48.5180010759625,-462.499999999992));
#33668=CARTESIAN_POINT('Ctrl Pts',(16.6597884011092,64.9397850479198,-439.572157057449));
#33669=CARTESIAN_POINT('Ctrl Pts',(16.6681713825567,64.9572515807444,-439.547770552181));
#33670=CARTESIAN_POINT('Ctrl Pts',(9.18299691544561,48.5070252542725,-462.548355953643));
#33671=CARTESIAN_POINT('Ctrl Pts',(9.20045900848171,48.5415610543782,-462.499999999992));
#33672=CARTESIAN_POINT('Ctrl Pts',(17.4800625805652,64.9166160566062,-439.572157057449));
#33673=CARTESIAN_POINT('Ctrl Pts',(17.4888689299737,64.9340328875783,-439.547770552181));
#33674=CARTESIAN_POINT('Ctrl Pts',(10.0217589312659,48.4668037795237,-462.548355953643));
#33675=CARTESIAN_POINT('Ctrl Pts',(10.0408892417922,48.5011082063693,-462.499999999992));
#33676=CARTESIAN_POINT('Ctrl Pts',(19.1114735664401,64.7664582111772,-439.572157057449));
#33677=CARTESIAN_POINT('Ctrl Pts',(19.1211212185536,64.7837583577536,-439.547770552181));
#33678=CARTESIAN_POINT('Ctrl Pts',(10.4389441100322,48.4029194680995,-462.548355953643));
#33679=CARTESIAN_POINT('Ctrl Pts',(10.4589027392674,48.4370911577441,-462.499999999992));
#33680=CARTESIAN_POINT('Ctrl Pts',(19.9222321103595,64.6395041823741,-439.572157057449));
#33681=CARTESIAN_POINT('Ctrl Pts',(19.9322974938387,64.6567373879391,-439.547770552181));
#33682=CARTESIAN_POINT('Ctrl Pts',(11.2431920479856,48.194304008609,-462.548355953643));
#33683=CARTESIAN_POINT('Ctrl Pts',(11.2648118978999,48.2281753266975,-462.499999999992));
#33684=CARTESIAN_POINT('Ctrl Pts',(21.5158045027278,64.288168000919,-439.572157057449));
#33685=CARTESIAN_POINT('Ctrl Pts',(21.5267076603337,64.3052497253947,-439.547770552181));
#33686=CARTESIAN_POINT('Ctrl Pts',(11.6301113843655,48.0496773411552,-462.548355953643));
#33687=CARTESIAN_POINT('Ctrl Pts',(11.6525644307871,48.0833808106781,-462.499999999992));
#33688=CARTESIAN_POINT('Ctrl Pts',(22.2986148768613,64.063788547369,-439.572157057449));
#33689=CARTESIAN_POINT('Ctrl Pts',(22.309938225767,64.0807856237378,-439.547770552181));
#33690=CARTESIAN_POINT('Ctrl Pts',(11.9917615758797,47.8725612702661,-462.548357991009));
#33691=CARTESIAN_POINT('Ctrl Pts',(12.0150531445734,47.9060664143383,-462.499999999992));
#33692=CARTESIAN_POINT('Ctrl Pts',(23.0586866286725,63.7924386819717,-439.571191046182));
#33693=CARTESIAN_POINT('Ctrl Pts',(23.0704328547269,63.8093357403638,-439.546803513444));
#33694=CARTESIAN_POINT('Ctrl Pts',(11.9948085870571,47.8710690143228,-462.548358008174));
#33695=CARTESIAN_POINT('Ctrl Pts',(12.0181072205521,47.9045724874437,-462.499999999992));
#33696=CARTESIAN_POINT('Ctrl Pts',(23.0650904608222,63.7901524780867,-439.571182907248));
#33697=CARTESIAN_POINT('Ctrl Pts',(23.0768402497433,63.8070486937973,-439.546795365853));
#33698=CARTESIAN_POINT('Ctrl Pts',(11.9978555982345,47.8695767583794,-462.548358025339));
#33699=CARTESIAN_POINT('Ctrl Pts',(12.0211612965308,47.903078560549,-462.499999999992));
#33700=CARTESIAN_POINT('Ctrl Pts',(23.0714942929719,63.7878662742018,-439.571174768313));
#33701=CARTESIAN_POINT('Ctrl Pts',(23.0832476447597,63.804761647231,-439.546787218263));
#33702=CARTESIAN_POINT('Ctrl Pts',(12.0009026094119,47.8680845024361,-462.548358042505));
#33703=CARTESIAN_POINT('Ctrl Pts',(12.0242153725094,47.9015846336544,-462.499999999992));
#33704=CARTESIAN_POINT('Ctrl Pts',(23.0778981251217,63.7855800703168,-439.571166629379));
#33705=CARTESIAN_POINT('Ctrl Pts',(23.0896550397761,63.8024746006646,-439.546779070672));
#33706=CARTESIAN_POINT('',(13.4208374317807,64.67554784793,-439.576815655849));
#33707=CARTESIAN_POINT('',(10.3755396625017,56.6085260457139,-450.759372645136));
#33708=CARTESIAN_POINT('Ctrl Pts',(23.0582397346381,63.7917958206654,-439.572118888233));
#33709=CARTESIAN_POINT('Ctrl Pts',(22.4761301356798,63.8565139964938,-439.738227128177));
#33710=CARTESIAN_POINT('Ctrl Pts',(20.5413879799313,64.0689664196242,-440.29417568351));
#33711=CARTESIAN_POINT('Ctrl Pts',(15.6870770962244,64.5124744893397,-440.37072762596));
#33712=CARTESIAN_POINT('Ctrl Pts',(13.9510385373826,64.6366301639263,-439.760738129923));
#33713=CARTESIAN_POINT('Ctrl Pts',(13.4208374317689,64.6755478479304,-439.576815655883));
#33714=CARTESIAN_POINT('Origin',(29.9999999999753,83.0468894509273,-439.));
#33715=CARTESIAN_POINT('',(10.6589034715959,64.8523969232218,-438.999999999994));
#33716=CARTESIAN_POINT('',(8.41281223346166,64.9597357704683,-438.999999999994));
#33717=CARTESIAN_POINT('Origin',(-0.00176539235111073,-134.670997806539,
-438.999999999971));
#33718=CARTESIAN_POINT('Ctrl Pts',(10.6589034715959,64.852396923219,-438.999999999998));
#33719=CARTESIAN_POINT('Ctrl Pts',(10.2791741653356,64.850135258153,-438.999999999998));
#33720=CARTESIAN_POINT('Ctrl Pts',(9.88830466079304,64.8595052145251,-438.999999999997));
#33721=CARTESIAN_POINT('Ctrl Pts',(9.15135256034744,64.8946619872636,-438.999999999997));
#33722=CARTESIAN_POINT('Ctrl Pts',(8.78144427771419,64.921756709229,-438.999999999998));
#33723=CARTESIAN_POINT('Ctrl Pts',(8.41281223346138,64.9597357704656,-438.999999999998));
#33724=CARTESIAN_POINT('Ctrl Pts',(2.49780576443942,48.2570143438195,-462.551779730762));
#33725=CARTESIAN_POINT('Ctrl Pts',(2.50499543252761,48.2947401420713,-462.499999999992));
#33726=CARTESIAN_POINT('Ctrl Pts',(5.76813712223451,65.4171752173726,-438.998971011752));
#33727=CARTESIAN_POINT('Ctrl Pts',(5.77258297236757,65.4405035884631,-438.966952159128));
#33728=CARTESIAN_POINT('Ctrl Pts',(2.50114805249965,48.2555045618294,-462.551779709936));
#33729=CARTESIAN_POINT('Ctrl Pts',(2.50834348888334,48.2932305351486,-462.499999999992));
#33730=CARTESIAN_POINT('Ctrl Pts',(5.77410320843019,65.4157450675561,-438.998980463695));
#33731=CARTESIAN_POINT('Ctrl Pts',(5.77855262548419,65.4390735469024,-438.966961623949));
#33732=CARTESIAN_POINT('Ctrl Pts',(2.50449034055988,48.253994779839,-462.551779689111));
#33733=CARTESIAN_POINT('Ctrl Pts',(2.51169154523912,48.2917209282259,-462.499999999992));
#33734=CARTESIAN_POINT('Ctrl Pts',(5.78006929462591,65.4143149177398,-438.998989915638));
#33735=CARTESIAN_POINT('Ctrl Pts',(5.7845222786008,65.4376435053419,-438.966971088769));
#33736=CARTESIAN_POINT('Ctrl Pts',(2.50783262862012,48.2524849978489,-462.551779668285));
#33737=CARTESIAN_POINT('Ctrl Pts',(2.51503960159485,48.2902113213033,-462.499999999992));
#33738=CARTESIAN_POINT('Ctrl Pts',(5.78603538082159,65.4128847679232,-438.99899936758));
#33739=CARTESIAN_POINT('Ctrl Pts',(5.79049193171741,65.4362134637813,-438.966980553589));
#33740=CARTESIAN_POINT('Ctrl Pts',(2.86166483944225,48.0926515275304,-462.551777463596));
#33741=CARTESIAN_POINT('Ctrl Pts',(2.86948247455032,48.1303963845574,-462.499999999992));
#33742=CARTESIAN_POINT('Ctrl Pts',(6.41763667626308,65.2614815787759,-438.999999999994));
#33743=CARTESIAN_POINT('Ctrl Pts',(6.42247084018541,65.2848217351751,-438.967982549309));
#33744=CARTESIAN_POINT('Ctrl Pts',(3.23771592613298,47.963840025296,-462.551777463596));
#33745=CARTESIAN_POINT('Ctrl Pts',(3.24611879784553,48.001598882328,-462.499999999992));
#33746=CARTESIAN_POINT('Ctrl Pts',(7.05989165386403,65.1390381946537,-438.999999999994));
#33747=CARTESIAN_POINT('Ctrl Pts',(7.0650877085168,65.1623870081876,-438.967982549309));
#33748=CARTESIAN_POINT('Ctrl Pts',(4.01580172662955,47.7814773668558,-462.551777463596));
#33749=CARTESIAN_POINT('Ctrl Pts',(4.02534345872193,47.8192291909888,-462.499999999992));
#33750=CARTESIAN_POINT('Ctrl Pts',(8.35600565353464,64.9534765136393,-438.999999999994));
#33751=CARTESIAN_POINT('Ctrl Pts',(8.36190594133271,64.9768209782635,-438.967982549309));
#33752=CARTESIAN_POINT('Ctrl Pts',(4.41771393105522,47.7279968672351,-462.551777463596));
#33753=CARTESIAN_POINT('Ctrl Pts',(4.42781120502764,47.7657432867869,-462.499999999992));
#33754=CARTESIAN_POINT('Ctrl Pts',(9.01061464568725,64.8975376569562,-438.999999999994));
#33755=CARTESIAN_POINT('Ctrl Pts',(9.01685846199188,64.9208787795684,-438.967982549309));
#33756=CARTESIAN_POINT('Ctrl Pts',(5.22431302604201,47.7018523564368,-462.551777463596));
#33757=CARTESIAN_POINT('Ctrl Pts',(5.23551978937467,47.7395377085665,-462.499999999992));
#33758=CARTESIAN_POINT('Ctrl Pts',(10.321882078837,64.8436156878735,-438.999999999994));
#33759=CARTESIAN_POINT('Ctrl Pts',(10.3288119662314,64.8669190484356,-438.967982549309));
#33760=CARTESIAN_POINT('Ctrl Pts',(5.62884640341604,47.7291960960751,-462.551777463596));
#33761=CARTESIAN_POINT('Ctrl Pts',(5.6406081038935,47.7668229830741,-462.499999999992));
#33762=CARTESIAN_POINT('Ctrl Pts',(10.9788371708056,64.8443656615973,-438.999999999994));
#33763=CARTESIAN_POINT('Ctrl Pts',(10.9861102127585,64.8676328692792,-438.967982549309));
#33764=CARTESIAN_POINT('Ctrl Pts',(6.41711316528365,47.8607864731195,-462.551777463596));
#33765=CARTESIAN_POINT('Ctrl Pts',(6.43001529825674,47.8982994369536,-462.499999999992));
#33766=CARTESIAN_POINT('Ctrl Pts',(12.2858472329501,64.9241363309766,-438.999999999994));
#33767=CARTESIAN_POINT('Ctrl Pts',(12.2938254801921,64.947333092386,-438.967982549309));
#33768=CARTESIAN_POINT('Ctrl Pts',(6.80072015482547,47.9649760744569,-462.551777463596));
#33769=CARTESIAN_POINT('Ctrl Pts',(6.8142082474083,48.0024123296618,-462.499999999992));
#33770=CARTESIAN_POINT('Ctrl Pts',(12.9359869834827,64.9934338298192,-438.999999999994));
#33771=CARTESIAN_POINT('Ctrl Pts',(12.9443275685373,65.0165831571792,-438.967982549309));
#33772=CARTESIAN_POINT('Ctrl Pts',(7.16416404091255,48.1015624851047,-462.551779701212));
#33773=CARTESIAN_POINT('Ctrl Pts',(7.17826498479954,48.1389160151653,-462.499999999992));
#33774=CARTESIAN_POINT('Ctrl Pts',(13.5781957322997,65.0923914334237,-438.998984423411));
#33775=CARTESIAN_POINT('Ctrl Pts',(13.5869152840909,65.1154896063231,-438.966965589059));
#33776=CARTESIAN_POINT('Ctrl Pts',(7.1675971205597,48.1028526760927,-462.551779722348));
#33777=CARTESIAN_POINT('Ctrl Pts',(7.18170385342104,48.1402054247342,-462.499999999992));
#33778=CARTESIAN_POINT('Ctrl Pts',(13.5842620161724,65.0933261838704,-438.998974830306));
#33779=CARTESIAN_POINT('Ctrl Pts',(13.5929851476715,65.1164238735664,-438.966955982884));
#33780=CARTESIAN_POINT('Ctrl Pts',(7.17103020020685,48.1041428670807,-462.551779743485));
#33781=CARTESIAN_POINT('Ctrl Pts',(7.18514272204257,48.1414948343031,-462.499999999992));
#33782=CARTESIAN_POINT('Ctrl Pts',(13.5903283000451,65.0942609343171,-438.998965237201));
#33783=CARTESIAN_POINT('Ctrl Pts',(13.5990550112522,65.1173581408096,-438.966946376709));
#33784=CARTESIAN_POINT('Ctrl Pts',(7.17446327985399,48.1054330580687,-462.551779764621));
#33785=CARTESIAN_POINT('Ctrl Pts',(7.18858159066407,48.1427842438719,-462.499999999992));
#33786=CARTESIAN_POINT('Ctrl Pts',(13.5963945839176,65.0951956847637,-438.998955644096));
#33787=CARTESIAN_POINT('Ctrl Pts',(13.6051248748329,65.1182924080529,-438.966936770534));
#33788=CARTESIAN_POINT('',(5.71602529916582,65.0464031681007,-439.501998174119));
#33789=CARTESIAN_POINT('',(4.11418572738962,56.6612575572247,-451.010674837211));
#33790=CARTESIAN_POINT('Ctrl Pts',(8.41281223346166,64.9597357704684,-438.999999999994));
#33791=CARTESIAN_POINT('Ctrl Pts',(8.00411492382587,64.9763677702042,-439.034050589004));
#33792=CARTESIAN_POINT('Ctrl Pts',(7.55093882802567,64.9931974319874,-439.093081656777));
#33793=CARTESIAN_POINT('Ctrl Pts',(6.38200340706734,65.0306627918092,-439.312440980534));
#33794=CARTESIAN_POINT('Ctrl Pts',(5.8858057335339,65.0423882666263,-439.453561504873));
#33795=CARTESIAN_POINT('Ctrl Pts',(5.71602529917806,65.0464031680998,-439.501998174162));
#33796=CARTESIAN_POINT('Ctrl Pts',(13.4208374317689,64.6755478479304,-439.576815655884));
#33797=CARTESIAN_POINT('Ctrl Pts',(13.1739140243162,64.6936335881493,-439.493381620575));
#33798=CARTESIAN_POINT('Ctrl Pts',(12.7545818536148,64.7244359742643,-439.352615648631));
#33799=CARTESIAN_POINT('Ctrl Pts',(11.6032651386067,64.7982807678147,-439.110697841396));
#33800=CARTESIAN_POINT('Ctrl Pts',(11.1446275207669,64.8257325793285,-439.040719881605));
#33801=CARTESIAN_POINT('Ctrl Pts',(10.658903471596,64.8523969232225,-438.999999999993));
#33802=CARTESIAN_POINT('Ctrl Pts',(-2.51803865109287,48.2556786139059,-462.541918531101));
#33803=CARTESIAN_POINT('Ctrl Pts',(-2.52389605211168,48.286218031592,-462.499999999992));
#33804=CARTESIAN_POINT('Ctrl Pts',(-5.7376033488292,65.0419001405148,-439.501081391007));
#33805=CARTESIAN_POINT('Ctrl Pts',(-5.74062486656665,65.0576537814102,-439.479457878315));
#33806=CARTESIAN_POINT('Ctrl Pts',(-2.51509415222326,48.2570089424155,-462.541918517992));
#33807=CARTESIAN_POINT('Ctrl Pts',(-2.52094390194258,48.2875491281623,-462.499999999992));
#33808=CARTESIAN_POINT('Ctrl Pts',(-5.73045325541913,65.0436526393717,-439.501088582933));
#33809=CARTESIAN_POINT('Ctrl Pts',(-5.73347082626322,65.0594066764682,-439.479465077003));
#33810=CARTESIAN_POINT('Ctrl Pts',(-2.51214965335364,48.2583392709251,-462.541918504884));
#33811=CARTESIAN_POINT('Ctrl Pts',(-2.51799175177345,48.2888802247325,-462.499999999992));
#33812=CARTESIAN_POINT('Ctrl Pts',(-5.72330316200906,65.0454051382286,-439.50109577486));
#33813=CARTESIAN_POINT('Ctrl Pts',(-5.72631678595981,65.0611595715262,-439.479472275692));
#33814=CARTESIAN_POINT('Ctrl Pts',(-2.50920515448402,48.2596695994346,-462.541918491776));
#33815=CARTESIAN_POINT('Ctrl Pts',(-2.51503960160435,48.2902113213028,-462.499999999992));
#33816=CARTESIAN_POINT('Ctrl Pts',(-5.71615306859899,65.0471576370855,-439.501102966786));
#33817=CARTESIAN_POINT('Ctrl Pts',(-5.7191627456564,65.0629124665843,-439.47947947438));
#33818=CARTESIAN_POINT('Ctrl Pts',(-2.12806987109674,48.4318670279101,-462.54191679505));
#33819=CARTESIAN_POINT('Ctrl Pts',(-2.1329139357002,48.4625081673819,-462.499999999992));
#33820=CARTESIAN_POINT('Ctrl Pts',(-4.79064655670577,65.2740007020806,-439.502033888159));
#33821=CARTESIAN_POINT('Ctrl Pts',(-4.79314534875941,65.2898068157669,-439.480411271002));
#33822=CARTESIAN_POINT('Ctrl Pts',(-1.72039652650194,48.5683071422839,-462.54191679505));
#33823=CARTESIAN_POINT('Ctrl Pts',(-1.72426166237677,48.5990124033193,-462.499999999992));
#33824=CARTESIAN_POINT('Ctrl Pts',(-3.84489764477392,65.4456857180531,-439.502033888159));
#33825=CARTESIAN_POINT('Ctrl Pts',(-3.8468914602163,65.4615249086009,-439.480411271002));
#33826=CARTESIAN_POINT('Ctrl Pts',(-0.875068093851045,48.7525347307723,
-462.54191679505));
#33827=CARTESIAN_POINT('Ctrl Pts',(-0.876992489635159,48.7833242476379,
-462.499999999992));
#33828=CARTESIAN_POINT('Ctrl Pts',(-1.93282676721124,65.6762251597991,-439.502033888159));
#33829=CARTESIAN_POINT('Ctrl Pts',(-1.93381945935864,65.6921078133922,-439.480411271002));
#33830=CARTESIAN_POINT('Ctrl Pts',(-0.437591237771207,48.8001901136637,
-462.54191679505));
#33831=CARTESIAN_POINT('Ctrl Pts',(-0.43855350484806,48.8309999999866,-462.499999999992));
#33832=CARTESIAN_POINT('Ctrl Pts',(-0.966508602396304,65.7350767687133,
-439.502033888159));
#33833=CARTESIAN_POINT('Ctrl Pts',(-0.96700498415872,65.7509699298123,-439.480411271002));
#33834=CARTESIAN_POINT('Ctrl Pts',(0.437591237761631,48.8001901136638,-462.54191679505));
#33835=CARTESIAN_POINT('Ctrl Pts',(0.438553504838485,48.8309999999867,-462.499999999992));
#33836=CARTESIAN_POINT('Ctrl Pts',(0.966508602384286,65.7350767687136,-439.502033888159));
#33837=CARTESIAN_POINT('Ctrl Pts',(0.967004984146674,65.7509699298127,-439.480411271002));
#33838=CARTESIAN_POINT('Ctrl Pts',(0.875068093841497,48.7525347307725,-462.54191679505));
#33839=CARTESIAN_POINT('Ctrl Pts',(0.876992489625583,48.7833242476381,-462.499999999992));
#33840=CARTESIAN_POINT('Ctrl Pts',(1.93282676719919,65.6762251597994,-439.502033888159));
#33841=CARTESIAN_POINT('Ctrl Pts',(1.93381945934659,65.6921078133925,-439.480411271002));
#33842=CARTESIAN_POINT('Ctrl Pts',(1.72039652649242,48.5683071422842,-462.54191679505));
#33843=CARTESIAN_POINT('Ctrl Pts',(1.72426166236725,48.5990124033196,-462.499999999992));
#33844=CARTESIAN_POINT('Ctrl Pts',(3.84489764476192,65.4456857180537,-439.502033888159));
#33845=CARTESIAN_POINT('Ctrl Pts',(3.84689146020431,65.4615249086015,-439.480411271002));
#33846=CARTESIAN_POINT('Ctrl Pts',(2.12806987108721,48.4318670279105,-462.54191679505));
#33847=CARTESIAN_POINT('Ctrl Pts',(2.1329139356907,48.4625081673823,-462.499999999992));
#33848=CARTESIAN_POINT('Ctrl Pts',(4.79064655669381,65.2740007020815,-439.502033888159));
#33849=CARTESIAN_POINT('Ctrl Pts',(4.79314534874745,65.2898068157678,-439.480411271002));
#33850=CARTESIAN_POINT('Ctrl Pts',(2.50920514799,48.2596697215709,-462.541918579872));
#33851=CARTESIAN_POINT('Ctrl Pts',(2.51503960159485,48.2902113213033,-462.499999999992));
#33852=CARTESIAN_POINT('Ctrl Pts',(5.71615662638683,65.0470906263832,-439.5010546324));
#33853=CARTESIAN_POINT('Ctrl Pts',(5.71916630678926,65.0628453928787,-439.47943109455));
#33854=CARTESIAN_POINT('Ctrl Pts',(2.5120017951438,48.2584061935381,-462.541918592968));
#33855=CARTESIAN_POINT('Ctrl Pts',(2.51784351590223,48.2889470628801,-462.499999999992));
#33856=CARTESIAN_POINT('Ctrl Pts',(5.72294771936374,65.0454256337786,-439.501047446939));
#33857=CARTESIAN_POINT('Ctrl Pts',(5.72596114849933,65.0611800235051,-439.479423902333));
#33858=CARTESIAN_POINT('Ctrl Pts',(2.51479844229763,48.2571426655051,-462.541918606065));
#33859=CARTESIAN_POINT('Ctrl Pts',(2.52064743020961,48.2876828044569,-462.499999999992));
#33860=CARTESIAN_POINT('Ctrl Pts',(5.72973881234068,65.0437606411741,-439.501040261477));
#33861=CARTESIAN_POINT('Ctrl Pts',(5.73275599020939,65.0595146541315,-439.479416710115));
#33862=CARTESIAN_POINT('Ctrl Pts',(2.51759508945143,48.2558791374724,-462.541918619161));
#33863=CARTESIAN_POINT('Ctrl Pts',(2.52345134451698,48.2864185460337,-462.499999999992));
#33864=CARTESIAN_POINT('Ctrl Pts',(5.73652990531762,65.0420956485695,-439.501033076016));
#33865=CARTESIAN_POINT('Ctrl Pts',(5.73955083191949,65.0578492847579,-439.479409517898));
#33866=CARTESIAN_POINT('',(-5.71602822336162,65.0465041066898,-439.501999936783));
#33867=CARTESIAN_POINT('',(-4.14907673705054,56.8439451514172,-450.760006334025));
#33868=CARTESIAN_POINT('Ctrl Pts',(5.71602529917836,65.0464031680999,-439.501998174162));
#33869=CARTESIAN_POINT('Ctrl Pts',(5.03832061887466,65.0623545154082,-439.699621167922));
#33870=CARTESIAN_POINT('Ctrl Pts',(2.84424303022636,65.1134462912443,-440.347752071002));
#33871=CARTESIAN_POINT('Ctrl Pts',(-2.84329574129294,65.1134990067166,-440.347698281527));
#33872=CARTESIAN_POINT('Ctrl Pts',(-5.03709134550615,65.0624738964574,-439.699899735949));
#33873=CARTESIAN_POINT('Ctrl Pts',(-5.71602822336464,65.0465041066898,-439.501999936793));
#33874=CARTESIAN_POINT('Origin',(29.9999999999753,83.0468894509273,-439.));
#33875=CARTESIAN_POINT('',(-8.41281803607202,64.9598843197978,-438.999999999994));
#33876=CARTESIAN_POINT('',(-10.6587895159293,64.8525916307611,-438.999999999994));
#33877=CARTESIAN_POINT('Origin',(-0.00176539235111073,-134.670997806539,
-438.999999999971));
#33878=CARTESIAN_POINT('Ctrl Pts',(-8.41281803607176,64.9598843197952,-438.999999999998));
#33879=CARTESIAN_POINT('Ctrl Pts',(-8.78383622403301,64.9216210322276,-438.999999999998));
#33880=CARTESIAN_POINT('Ctrl Pts',(-9.15614215981989,64.8943339071276,-438.999999999998));
#33881=CARTESIAN_POINT('Ctrl Pts',(-9.89456730134841,64.8593136998998,-438.999999999998));
#33882=CARTESIAN_POINT('Ctrl Pts',(-10.2814664621786,64.8502517844627,-438.999999999998));
#33883=CARTESIAN_POINT('Ctrl Pts',(-10.6587895159293,64.8525916307586,-438.999999999998));
#33884=CARTESIAN_POINT('Ctrl Pts',(-7.17446331057034,48.1054326881418,-462.551779506093));
#33885=CARTESIAN_POINT('Ctrl Pts',(-7.18858159067015,48.1427842438694,-462.499999999992));
#33886=CARTESIAN_POINT('Ctrl Pts',(-13.5963806453087,65.0953635799082,-438.999072982214));
#33887=CARTESIAN_POINT('Ctrl Pts',(-13.6047828789584,65.1175926684504,-438.968257365478));
#33888=CARTESIAN_POINT('Ctrl Pts',(-7.1710302306422,48.1041425005522,-462.551779487331));
#33889=CARTESIAN_POINT('Ctrl Pts',(-7.18514272204976,48.1414948343009,-462.499999999992));
#33890=CARTESIAN_POINT('Ctrl Pts',(-13.5903144894735,65.0944272872329,-438.99908149749));
#33891=CARTESIAN_POINT('Ctrl Pts',(-13.5987132780899,65.1166568388001,-438.96826589192));
#33892=CARTESIAN_POINT('Ctrl Pts',(-7.16759715071408,48.1028523129626,-462.551779468569));
#33893=CARTESIAN_POINT('Ctrl Pts',(-7.18170385342937,48.1402054247325,-462.499999999992));
#33894=CARTESIAN_POINT('Ctrl Pts',(-13.5842483336382,65.0934909945578,-438.999090012766));
#33895=CARTESIAN_POINT('Ctrl Pts',(-13.5926436772213,65.1157210091498,-438.968274418361));
#33896=CARTESIAN_POINT('Ctrl Pts',(-7.16416407078593,48.101562125373,-462.551779449808));
#33897=CARTESIAN_POINT('Ctrl Pts',(-7.17826498480897,48.138916015164,-462.499999999992));
#33898=CARTESIAN_POINT('Ctrl Pts',(-13.578182177803,65.0925547018826,-438.999098528042));
#33899=CARTESIAN_POINT('Ctrl Pts',(-13.5865740763529,65.1147851794995,-438.968282944803));
#33900=CARTESIAN_POINT('Ctrl Pts',(-6.80072015483429,47.9649760744541,-462.551777463598));
#33901=CARTESIAN_POINT('Ctrl Pts',(-6.81420824741771,48.0024123296606,-462.499999999992));
#33902=CARTESIAN_POINT('Ctrl Pts',(-12.9359869834945,64.9934338298169,-438.999999999994));
#33903=CARTESIAN_POINT('Ctrl Pts',(-12.9440141726828,65.0157133256896,-438.969185598811));
#33904=CARTESIAN_POINT('Ctrl Pts',(-6.41711316529248,47.8607864731167,-462.551777463598));
#33905=CARTESIAN_POINT('Ctrl Pts',(-6.43001529826615,47.8982994369525,-462.499999999992));
#33906=CARTESIAN_POINT('Ctrl Pts',(-12.2858472329619,64.9241363309746,-438.999999999994));
#33907=CARTESIAN_POINT('Ctrl Pts',(-12.2935256991105,64.9464614785712,-438.969185598811));
#33908=CARTESIAN_POINT('Ctrl Pts',(-5.62884641196265,47.7291951231673,-462.551777463598));
#33909=CARTESIAN_POINT('Ctrl Pts',(-5.64060810390288,47.7668229830731,-462.499999999992));
#33910=CARTESIAN_POINT('Ctrl Pts',(-10.9788332958342,64.844807229598,-438.999999999994));
#33911=CARTESIAN_POINT('Ctrl Pts',(-10.9858330495647,64.8672007554688,-438.969185598811));
#33912=CARTESIAN_POINT('Ctrl Pts',(-5.22431302605086,47.7018523564343,-462.551777463598));
#33913=CARTESIAN_POINT('Ctrl Pts',(-5.23551978938402,47.7395377085656,-462.499999999992));
#33914=CARTESIAN_POINT('Ctrl Pts',(-10.3218820788488,64.8436156878717,-438.999999999994));
#33915=CARTESIAN_POINT('Ctrl Pts',(-10.3285515770679,64.8660434291788,-438.969185598811));
#33916=CARTESIAN_POINT('Ctrl Pts',(-4.41771393106416,47.7279968672327,-462.551777463598));
#33917=CARTESIAN_POINT('Ctrl Pts',(-4.42781120503702,47.7657432867861,-462.499999999992));
#33918=CARTESIAN_POINT('Ctrl Pts',(-9.01061464569913,64.8975376569547,-438.999999999994));
#33919=CARTESIAN_POINT('Ctrl Pts',(-9.01662385181665,64.92000174141,-438.969185598811));
#33920=CARTESIAN_POINT('Ctrl Pts',(-4.01580166730864,47.7814767988564,-462.551777463598));
#33921=CARTESIAN_POINT('Ctrl Pts',(-4.02534345873132,47.8192291909881,-462.499999999992));
#33922=CARTESIAN_POINT('Ctrl Pts',(-8.35603258132023,64.9537343079005,-438.999999999994));
#33923=CARTESIAN_POINT('Ctrl Pts',(-8.36171120225726,64.9762019468255,-438.969185598811));
#33924=CARTESIAN_POINT('Ctrl Pts',(-3.237715926142,47.9638400252938,-462.551777463598));
#33925=CARTESIAN_POINT('Ctrl Pts',(-3.24611879785494,48.0015988823275,-462.499999999992));
#33926=CARTESIAN_POINT('Ctrl Pts',(-7.05989165387597,65.1390381946525,-438.999999999994));
#33927=CARTESIAN_POINT('Ctrl Pts',(-7.06489246778255,65.1615096810445,-438.969185598811));
#33928=CARTESIAN_POINT('Ctrl Pts',(-2.86166483945136,48.0926515275283,-462.551777463598));
#33929=CARTESIAN_POINT('Ctrl Pts',(-2.86948247455976,48.1303963845569,-462.499999999992));
#33930=CARTESIAN_POINT('Ctrl Pts',(-6.41763667627501,65.2614815787748,-438.999999999994));
#33931=CARTESIAN_POINT('Ctrl Pts',(-6.42228919742521,65.2839447333224,-438.969185598811));
#33932=CARTESIAN_POINT('Ctrl Pts',(-2.50783263663928,48.2524848469793,-462.551779559468));
#33933=CARTESIAN_POINT('Ctrl Pts',(-2.51503960160435,48.2902113213028,-462.499999999992));
#33934=CARTESIAN_POINT('Ctrl Pts',(-5.78603174536888,65.4129532414351,-438.999048757082));
#33935=CARTESIAN_POINT('Ctrl Pts',(-5.79032083746175,65.4354054558553,-438.968233108581));
#33936=CARTESIAN_POINT('Ctrl Pts',(-2.50449034865332,48.253994627545,-462.551779579265));
#33937=CARTESIAN_POINT('Ctrl Pts',(-2.51169154524722,48.2917209282261,-462.499999999992));
#33938=CARTESIAN_POINT('Ctrl Pts',(-5.78006562483024,65.4143840380509,-438.999039771671));
#33939=CARTESIAN_POINT('Ctrl Pts',(-5.78435128398358,65.4368361491308,-438.968224111388));
#33940=CARTESIAN_POINT('Ctrl Pts',(-2.5011480606674,48.2555044081108,-462.551779599063));
#33941=CARTESIAN_POINT('Ctrl Pts',(-2.50834348889009,48.2932305351494,-462.499999999992));
#33942=CARTESIAN_POINT('Ctrl Pts',(-5.77409950429161,65.4158148346665,-438.99903078626));
#33943=CARTESIAN_POINT('Ctrl Pts',(-5.77838173050535,65.4382668424065,-438.968215114195));
#33944=CARTESIAN_POINT('Ctrl Pts',(-2.49780577268147,48.2570141886766,-462.551779618861));
#33945=CARTESIAN_POINT('Ctrl Pts',(-2.50499543253297,48.2947401420728,-462.499999999992));
#33946=CARTESIAN_POINT('Ctrl Pts',(-5.76813338375298,65.4172456312822,-438.999021800849));
#33947=CARTESIAN_POINT('Ctrl Pts',(-5.77241217702715,65.4396975356821,-438.968206117001));
#33948=CARTESIAN_POINT('',(-13.4208533932044,64.6757844080299,-439.576819794402));
#33949=CARTESIAN_POINT('',(-10.2970852952296,56.400796767239,-451.047494191925));
#33950=CARTESIAN_POINT('Ctrl Pts',(-10.6587895159293,64.8525916307614,-438.999999999994));
#33951=CARTESIAN_POINT('Ctrl Pts',(-11.1431746641298,64.8260069038297,-439.040765404272));
#33952=CARTESIAN_POINT('Ctrl Pts',(-11.6025803817587,64.7985306170646,-439.11052042917));
#33953=CARTESIAN_POINT('Ctrl Pts',(-12.7544621947915,64.7246760613877,-439.352217793466));
#33954=CARTESIAN_POINT('Ctrl Pts',(-13.1700622987402,64.6941515478973,-439.491932720156));
#33955=CARTESIAN_POINT('Ctrl Pts',(-13.4208533931901,64.6757844080304,-439.576819794444));
#33956=CARTESIAN_POINT('Ctrl Pts',(-5.71602822336486,65.0465041066897,-439.501999936794));
#33957=CARTESIAN_POINT('Ctrl Pts',(-5.88573707745702,65.04249459091,-439.45354399244));
#33958=CARTESIAN_POINT('Ctrl Pts',(-6.38201999480569,65.0307778175158,-439.312278964639));
#33959=CARTESIAN_POINT('Ctrl Pts',(-7.55211977412035,64.993294425775,-439.092788088094));
#33960=CARTESIAN_POINT('Ctrl Pts',(-8.00524379523663,64.9764622470322,-439.034023415792));
#33961=CARTESIAN_POINT('Ctrl Pts',(-8.41281803607201,64.9598843197981,-438.999999999994));
#33962=CARTESIAN_POINT('Ctrl Pts',(-12.001137535198,47.8672571975149,-462.54912382016));
#33963=CARTESIAN_POINT('Ctrl Pts',(-12.0248210021412,47.9012883848401,-462.499999999992));
#33964=CARTESIAN_POINT('Ctrl Pts',(-23.079130834684,63.7854192666133,-439.571349832351));
#33965=CARTESIAN_POINT('Ctrl Pts',(-23.0913829153359,63.8030244953067,-439.545936787544));
#33966=CARTESIAN_POINT('Ctrl Pts',(-11.9978892331025,47.8688480698695,-462.549123805034));
#33967=CARTESIAN_POINT('Ctrl Pts',(-12.0215650496218,47.9028810613388,-462.499999999992));
#33968=CARTESIAN_POINT('Ctrl Pts',(-23.0723040300149,63.787854031318,-439.571356892768));
#33969=CARTESIAN_POINT('Ctrl Pts',(-23.0845521529011,63.8054601933426,-439.545943855786));
#33970=CARTESIAN_POINT('Ctrl Pts',(-11.9946409310072,47.8704389422241,-462.549123789907));
#33971=CARTESIAN_POINT('Ctrl Pts',(-12.0183090971022,47.9044737378375,-462.499999999992));
#33972=CARTESIAN_POINT('Ctrl Pts',(-23.065477225346,63.7902887960227,-439.571363953185));
#33973=CARTESIAN_POINT('Ctrl Pts',(-23.0777213904665,63.8078958913785,-439.545950924028));
#33974=CARTESIAN_POINT('Ctrl Pts',(-11.9913926289119,47.8720298145787,-462.54912377478));
#33975=CARTESIAN_POINT('Ctrl Pts',(-12.0150531445829,47.9060664143362,-462.499999999992));
#33976=CARTESIAN_POINT('Ctrl Pts',(-23.0586504206769,63.7927235607274,-439.571371013602));
#33977=CARTESIAN_POINT('Ctrl Pts',(-23.0708906280318,63.8103315894145,-439.545957992271));
#33978=CARTESIAN_POINT('Ctrl Pts',(-11.6297556451161,48.0491433536022,-462.549122090709));
#33979=CARTESIAN_POINT('Ctrl Pts',(-11.6525644307966,48.083380810676,-462.499999999992));
#33980=CARTESIAN_POINT('Ctrl Pts',(-22.2986148768729,64.0637885473651,-439.572157057449));
#33981=CARTESIAN_POINT('Ctrl Pts',(-22.3104144618915,64.0815004848273,-439.546744907332));
#33982=CARTESIAN_POINT('Ctrl Pts',(-11.242849509649,48.1937673617144,-462.549122090709));
#33983=CARTESIAN_POINT('Ctrl Pts',(-11.2648118979094,48.2281753266956,-462.499999999992));
#33984=CARTESIAN_POINT('Ctrl Pts',(-21.5158045027396,64.2881680009153,-439.572157057449));
#33985=CARTESIAN_POINT('Ctrl Pts',(-21.5271662241007,64.3059681466046,-439.546744907332));
#33986=CARTESIAN_POINT('Ctrl Pts',(-10.4386278915723,48.4023780622091,-462.549122090709));
#33987=CARTESIAN_POINT('Ctrl Pts',(-10.4589027392768,48.4370911577423,-462.499999999992));
#33988=CARTESIAN_POINT('Ctrl Pts',(-19.9222321103714,64.6395041823707,-439.572157057449));
#33989=CARTESIAN_POINT('Ctrl Pts',(-19.9327208225974,64.6574621801238,-439.546744907332));
#33990=CARTESIAN_POINT('Ctrl Pts',(-10.0214566187051,48.4662722784951,-462.549122090709));
#33991=CARTESIAN_POINT('Ctrl Pts',(-10.040890022398,48.5011201886057,-462.499999999992));
#33992=CARTESIAN_POINT('Ctrl Pts',(-19.111473566452,64.7664582111738,-439.572157057449));
#33993=CARTESIAN_POINT('Ctrl Pts',(-19.1215269775492,64.7844859520552,-439.546744907332));
#33994=CARTESIAN_POINT('Ctrl Pts',(-9.18272025134817,48.5064780795265,-462.549122090709));
#33995=CARTESIAN_POINT('Ctrl Pts',(-9.2004590084912,48.5415610543766,-462.499999999992));
#33996=CARTESIAN_POINT('Ctrl Pts',(-17.4800625805772,64.9166160566032,-439.572157057449));
#33997=CARTESIAN_POINT('Ctrl Pts',(-17.4892393064215,64.9347654026598,-439.546744907332));
#33998=CARTESIAN_POINT('Ctrl Pts',(-8.76134336058432,48.4828179859497,-462.549122090709));
#33999=CARTESIAN_POINT('Ctrl Pts',(-8.77822932151279,48.518001075961,-462.499999999992));
#34000=CARTESIAN_POINT('Ctrl Pts',(-16.6597884011211,64.9397850479169,-439.572157057449));
#34001=CARTESIAN_POINT('Ctrl Pts',(-16.6685239530432,64.9579861861807,-439.546744907332));
#34002=CARTESIAN_POINT('Ctrl Pts',(-7.94082488447429,48.3521211537968,-462.549122090709));
#34003=CARTESIAN_POINT('Ctrl Pts',(-7.95597858419148,48.3874670903318,-462.499999999992));
#34004=CARTESIAN_POINT('Ctrl Pts',(-15.0290009666032,64.8852600322724,-439.572157057449));
#34005=CARTESIAN_POINT('Ctrl Pts',(-15.0368403742184,64.903545415328,-439.546744907332));
#34006=CARTESIAN_POINT('Ctrl Pts',(-7.5418363068398,48.2451812560949,-462.549122090709));
#34007=CARTESIAN_POINT('Ctrl Pts',(-7.55611022239511,48.280589721988,-462.499999999992));
#34008=CARTESIAN_POINT('Ctrl Pts',(-14.218491429066,64.8075683781914,-439.572157057449));
#34009=CARTESIAN_POINT('Ctrl Pts',(-14.2258757011838,64.8258861093293,-439.546744907332));
#34010=CARTESIAN_POINT('Ctrl Pts',(-7.16488722681163,48.1034777948425,-462.549123975058));
#34011=CARTESIAN_POINT('Ctrl Pts',(-7.17826498480897,48.138916015164,-462.499999999992));
#34012=CARTESIAN_POINT('Ctrl Pts',(-13.4223626974158,64.6797826157486,-439.571277533733));
#34013=CARTESIAN_POINT('Ctrl Pts',(-13.4292833636476,64.6981157396354,-439.545864408792));
#34014=CARTESIAN_POINT('Ctrl Pts',(-7.16167302984563,48.1022695074123,-462.549123991125));
#34015=CARTESIAN_POINT('Ctrl Pts',(-7.1750431464212,48.1377079814461,-462.499999999992));
#34016=CARTESIAN_POINT('Ctrl Pts',(-13.4155742087594,64.6786930027698,-439.571270034146));
#34017=CARTESIAN_POINT('Ctrl Pts',(-13.4224909218826,64.6970262579086,-439.545856900893));
#34018=CARTESIAN_POINT('Ctrl Pts',(-7.15845883287963,48.101061219982,-462.549124007193));
#34019=CARTESIAN_POINT('Ctrl Pts',(-7.17182130803346,48.1364999477281,-462.499999999992));
#34020=CARTESIAN_POINT('Ctrl Pts',(-13.408785720103,64.677603389791,-439.571262534558));
#34021=CARTESIAN_POINT('Ctrl Pts',(-13.4156984801177,64.6959367761818,-439.545849392994));
#34022=CARTESIAN_POINT('Ctrl Pts',(-7.15524463591363,48.0998529325518,-462.54912402326));
#34023=CARTESIAN_POINT('Ctrl Pts',(-7.16859946964568,48.1352919140101,-462.499999999992));
#34024=CARTESIAN_POINT('Ctrl Pts',(-13.4019972314466,64.6765137768122,-439.571255034971));
#34025=CARTESIAN_POINT('Ctrl Pts',(-13.4089060383527,64.6948472944551,-439.545841885095));
#34026=CARTESIAN_POINT('',(-23.0582867813677,63.7922004510104,-439.572125998435));
#34027=CARTESIAN_POINT('',(-17.67449156409,56.0473953277366,-450.749918885292));
#34028=CARTESIAN_POINT('Ctrl Pts',(-13.4208533931897,64.6757844080304,-439.576819794444));
#34029=CARTESIAN_POINT('Ctrl Pts',(-13.9566749456381,64.6364685998891,-439.76241002145));
#34030=CARTESIAN_POINT('Ctrl Pts',(-15.6979001875856,64.5119662151012,-440.373416758168));
#34031=CARTESIAN_POINT('Ctrl Pts',(-20.5490919569703,64.0684585284553,-440.290614638996));
#34032=CARTESIAN_POINT('Ctrl Pts',(-22.4739368675365,63.8571630490881,-439.738547054618));
#34033=CARTESIAN_POINT('Ctrl Pts',(-23.0582867814246,63.7922004510004,-439.572125998638));
#34034=CARTESIAN_POINT('Origin',(29.9999999999753,83.0468894509273,-439.));
#34035=CARTESIAN_POINT('',(-26.1597137411461,63.4173578413804,-438.999999999994));
#34036=CARTESIAN_POINT('',(-28.3882768422949,63.1102977520074,-438.999999999994));
#34037=CARTESIAN_POINT('Origin',(-0.00176539235111073,-134.670997806539,
-438.999999999971));
#34038=CARTESIAN_POINT('Ctrl Pts',(-26.1597137411455,63.4173578413776,-438.999999999997));
#34039=CARTESIAN_POINT('Ctrl Pts',(-26.5275732374657,63.3451801861953,-438.999999999997));
#34040=CARTESIAN_POINT('Ctrl Pts',(-26.8973783983544,63.2833853100965,-438.999999999934));
#34041=CARTESIAN_POINT('Ctrl Pts',(-27.6412583367134,63.1808107453415,-438.999999999934));
#34042=CARTESIAN_POINT('Ctrl Pts',(-28.0144149229582,63.140261967893,-438.999999999997));
#34043=CARTESIAN_POINT('Ctrl Pts',(-28.3882768422946,63.1102977520047,-438.999999999997));
#34044=CARTESIAN_POINT('Ctrl Pts',(-18.8775059186204,47.6342738478878,-462.508833269478));
#34045=CARTESIAN_POINT('Ctrl Pts',(-18.8849353455675,47.6408044887233,-462.499999999992));
#34046=CARTESIAN_POINT('Ctrl Pts',(-38.6501574445149,65.0148990831144,-438.999999999994));
#34047=CARTESIAN_POINT('Ctrl Pts',(-38.6570457183015,65.0209540376077,-438.991810138368));
#34048=CARTESIAN_POINT('Ctrl Pts',(-18.8753643113511,47.6334276618779,-462.508833269478));
#34049=CARTESIAN_POINT('Ctrl Pts',(-18.8827928271309,47.6399577985274,-462.499999999992));
#34050=CARTESIAN_POINT('Ctrl Pts',(-38.6455908591808,65.0127110581453,-438.999999999994));
#34051=CARTESIAN_POINT('Ctrl Pts',(-38.6524782881685,65.0187655451771,-438.991810138368));
#34052=CARTESIAN_POINT('Ctrl Pts',(-18.873222704082,47.632581475868,-462.508833269478));
#34053=CARTESIAN_POINT('Ctrl Pts',(-18.8806503086941,47.6391111083315,-462.499999999992));
#34054=CARTESIAN_POINT('Ctrl Pts',(-38.6410242738467,65.0105230331761,-438.999999999994));
#34055=CARTESIAN_POINT('Ctrl Pts',(-38.6479108580357,65.0165770527465,-438.991810138368));
#34056=CARTESIAN_POINT('Ctrl Pts',(-18.8710810968126,47.6317352898581,-462.508833269478));
#34057=CARTESIAN_POINT('Ctrl Pts',(-18.8785077902573,47.6382644181355,-462.499999999992));
#34058=CARTESIAN_POINT('Ctrl Pts',(-38.6364576885126,65.008335008207,-438.999999999994));
#34059=CARTESIAN_POINT('Ctrl Pts',(-38.6433434279027,65.0143885603157,-438.991810138368));
#34060=CARTESIAN_POINT('Ctrl Pts',(-18.6207111444172,47.5328097986826,-462.508833269478));
#34061=CARTESIAN_POINT('Ctrl Pts',(-18.6280313155475,47.5392799838325,-462.499999999992));
#34062=CARTESIAN_POINT('Ctrl Pts',(-38.1025896123615,64.7525384785492,-438.999999999994));
#34063=CARTESIAN_POINT('Ctrl Pts',(-38.1093765884324,64.7585373808978,-438.991810138368));
#34064=CARTESIAN_POINT('Ctrl Pts',(-18.3668172652831,47.4458875093331,-462.508833269478));
#34065=CARTESIAN_POINT('Ctrl Pts',(-18.3740287411124,47.4523034520998,-462.499999999992));
#34066=CARTESIAN_POINT('Ctrl Pts',(-37.5594144298113,64.5212556955974,-438.999999999994));
#34067=CARTESIAN_POINT('Ctrl Pts',(-37.5661006278547,64.527204306532,-438.991810138368));
#34068=CARTESIAN_POINT('Ctrl Pts',(-17.3709360911557,47.1570554700231,-462.508833269478));
#34069=CARTESIAN_POINT('Ctrl Pts',(-17.377718225807,47.1632792121921,-462.499999999992));
#34070=CARTESIAN_POINT('Ctrl Pts',(-35.420886109377,63.7209016414593,-438.999999999994));
#34071=CARTESIAN_POINT('Ctrl Pts',(-35.4271742390897,63.7266720515249,-438.991810138368));
#34072=CARTESIAN_POINT('Ctrl Pts',(-16.616292128253,47.0488954908114,-462.508833269478));
#34073=CARTESIAN_POINT('Ctrl Pts',(-16.6227423732312,47.0550172977463,-462.499999999992));
#34074=CARTESIAN_POINT('Ctrl Pts',(-33.7829521032343,63.3414515779963,-438.999999999994));
#34075=CARTESIAN_POINT('Ctrl Pts',(-33.7889325178365,63.3471274777037,-438.991810138368));
#34076=CARTESIAN_POINT('Ctrl Pts',(-15.1578028767041,47.0244381605313,-462.508833269478));
#34077=CARTESIAN_POINT('Ctrl Pts',(-15.1635931228177,47.0304369741045,-462.499999999992));
#34078=CARTESIAN_POINT('Ctrl Pts',(-30.5679441254776,62.9896601345508,-438.999999999994));
#34079=CARTESIAN_POINT('Ctrl Pts',(-30.5733126149729,62.9952219996288,-438.991810138368));
#34080=CARTESIAN_POINT('Ctrl Pts',(-14.4544087306705,47.1073598914834,-462.50883327605));
#34081=CARTESIAN_POINT('Ctrl Pts',(-14.4598710640638,47.1133367987068,-462.499999999992));
#34082=CARTESIAN_POINT('Ctrl Pts',(-28.9918441848079,63.0142803808168,-438.999982515861));
#34083=CARTESIAN_POINT('Ctrl Pts',(-28.9969086464675,63.0198219351849,-438.991792648143));
#34084=CARTESIAN_POINT('Ctrl Pts',(-13.1507400659786,47.4134699086769,-462.508833253297));
#34085=CARTESIAN_POINT('Ctrl Pts',(-13.1555740488444,47.4194722561782,-462.499999999992));
#34086=CARTESIAN_POINT('Ctrl Pts',(-26.0158855700949,63.3880970670556,-439.000043049088));
#34087=CARTESIAN_POINT('Ctrl Pts',(-26.0203674497467,63.3936622086534,-438.991853202466));
#34088=CARTESIAN_POINT('Ctrl Pts',(-12.5503158851177,47.6359705084204,-462.508833269478));
#34089=CARTESIAN_POINT('Ctrl Pts',(-12.5548498814442,47.6420203105473,-462.499999999992));
#34090=CARTESIAN_POINT('Ctrl Pts',(-24.6170782372607,63.7368932453249,-438.999999999994));
#34091=CARTESIAN_POINT('Ctrl Pts',(-24.6212819811383,63.7425023849935,-438.991810138368));
#34092=CARTESIAN_POINT('Ctrl Pts',(-12.0107984455655,47.899945859334,-462.508833572313));
#34093=CARTESIAN_POINT('Ctrl Pts',(-12.0150531445829,47.9060664143362,-462.499999999992));
#34094=CARTESIAN_POINT('Ctrl Pts',(-23.3342398922659,64.1891700571751,-438.999194340672));
#34095=CARTESIAN_POINT('Ctrl Pts',(-23.3381846826136,64.1948447961396,-438.99100419827));
#34096=CARTESIAN_POINT('Ctrl Pts',(-12.0091656235255,47.9007447672828,-462.508833573229));
#34097=CARTESIAN_POINT('Ctrl Pts',(-12.0134194772637,47.906865536415,-462.499999999992));
#34098=CARTESIAN_POINT('Ctrl Pts',(-23.3303574473811,64.1905388499007,-438.999191902385));
#34099=CARTESIAN_POINT('Ctrl Pts',(-23.3343014540193,64.1962137873981,-438.991001759134));
#34100=CARTESIAN_POINT('Ctrl Pts',(-12.0075328014854,47.9015436752317,-462.508833574146));
#34101=CARTESIAN_POINT('Ctrl Pts',(-12.0117858099447,47.9076646584938,-462.499999999992));
#34102=CARTESIAN_POINT('Ctrl Pts',(-23.3264750024962,64.1919076426262,-438.999189464098));
#34103=CARTESIAN_POINT('Ctrl Pts',(-23.3304182254248,64.1975827786566,-438.990999319997));
#34104=CARTESIAN_POINT('Ctrl Pts',(-12.0058999794455,47.9023425831805,-462.508833575062));
#34105=CARTESIAN_POINT('Ctrl Pts',(-12.0101521426257,47.9084637805726,-462.499999999992));
#34106=CARTESIAN_POINT('Ctrl Pts',(-23.3225925576115,64.1932764353518,-438.999187025811));
#34107=CARTESIAN_POINT('Ctrl Pts',(-23.3265349968304,64.198951769915,-438.99099688086));
#34108=CARTESIAN_POINT('',(-33.4829940324908,62.2764393526616,-440.999972026227));
#34109=CARTESIAN_POINT('Ctrl Pts',(-33.4829940630133,62.2764393583309,-440.9999720502));
#34110=CARTESIAN_POINT('Ctrl Pts',(-31.1113726356467,59.8388581046014,-444.596060591447));
#34111=CARTESIAN_POINT('Ctrl Pts',(-28.6868186804599,57.3709516983183,-448.232584923789));
#34112=CARTESIAN_POINT('Ctrl Pts',(-23.4113303313584,52.0741661663874,-456.017611271358));
#34113=CARTESIAN_POINT('Ctrl Pts',(-21.3792166372997,50.0678629208131,-458.957669002678));
#34114=CARTESIAN_POINT('Ctrl Pts',(-18.878507790257,47.6382644181356,-462.499999999992));
#34115=CARTESIAN_POINT('Ctrl Pts',(-28.3882768422949,63.1102977520076,-438.999999999993));
#34116=CARTESIAN_POINT('Ctrl Pts',(-29.3116124609106,62.9763196718963,-439.082600088505));
#34117=CARTESIAN_POINT('Ctrl Pts',(-30.2271255160582,62.8347324864127,-439.274916650434));
#34118=CARTESIAN_POINT('Ctrl Pts',(-32.180534929123,62.5140220534877,-440.010156560329));
#34119=CARTESIAN_POINT('Ctrl Pts',(-32.9450987460992,62.3760920008183,-440.536273886144));
#34120=CARTESIAN_POINT('Ctrl Pts',(-33.482994016876,62.2764393498852,-440.999972043744));
#34121=CARTESIAN_POINT('Ctrl Pts',(-23.0582867814239,63.7922004510005,-439.572125998639));
#34122=CARTESIAN_POINT('Ctrl Pts',(-23.2597393793474,63.7697900102401,-439.515595788428));
#34123=CARTESIAN_POINT('Ctrl Pts',(-23.8404446999355,63.7050803487465,-439.353219756612));
#34124=CARTESIAN_POINT('Ctrl Pts',(-25.1137024112667,63.5513262928731,-439.115720930552));
#34125=CARTESIAN_POINT('Ctrl Pts',(-25.6361613101107,63.4857267740936,-439.04357303287));
#34126=CARTESIAN_POINT('Ctrl Pts',(-26.1597137411461,63.4173578413807,-438.999999999993));
#34127=CARTESIAN_POINT('Ctrl Pts',(-42.0325401995064,60.6377891214161,-440.991114438282));
#34128=CARTESIAN_POINT('Ctrl Pts',(-42.0285040216223,60.6317485621414,-440.999646067766));
#34129=CARTESIAN_POINT('Ctrl Pts',(-31.8570244760066,45.4090817011473,-462.499999999992));
#34130=CARTESIAN_POINT('Ctrl Pts',(-31.8468530089389,45.3938590466631,-462.521500335317));
#34131=CARTESIAN_POINT('Ctrl Pts',(-42.0051853072238,60.6436503983426,-440.99111632347));
#34132=CARTESIAN_POINT('Ctrl Pts',(-42.0011517636324,60.6376092981949,-440.999647949747));
#34133=CARTESIAN_POINT('Ctrl Pts',(-31.8363095381066,45.413574653915,-462.499999999992));
#34134=CARTESIAN_POINT('Ctrl Pts',(-31.8261447041996,45.3983506275219,-462.521500339637));
#34135=CARTESIAN_POINT('Ctrl Pts',(-41.9778304149411,60.6495116752692,-440.991118208659));
#34136=CARTESIAN_POINT('Ctrl Pts',(-41.9737995056426,60.6434700342484,-440.999649831728));
#34137=CARTESIAN_POINT('Ctrl Pts',(-31.8155946002065,45.4180676066827,-462.499999999992));
#34138=CARTESIAN_POINT('Ctrl Pts',(-31.8054363994604,45.4028422083807,-462.521500343958));
#34139=CARTESIAN_POINT('Ctrl Pts',(-41.9504755226585,60.6553729521959,-440.991120093849));
#34140=CARTESIAN_POINT('Ctrl Pts',(-41.9464472476527,60.6493307703021,-440.999651713709));
#34141=CARTESIAN_POINT('Ctrl Pts',(-31.7948796623065,45.4225605594505,-462.499999999992));
#34142=CARTESIAN_POINT('Ctrl Pts',(-31.7847280947211,45.4073337892395,-462.521500348278));
#34143=CARTESIAN_POINT('Ctrl Pts',(-36.316732701322,61.8625035257008,-440.991508348712));
#34144=CARTESIAN_POINT('Ctrl Pts',(-36.3132469591819,61.8563499509359,-441.000039307893));
#34145=CARTESIAN_POINT('Ctrl Pts',(-27.5283826319057,46.3479396136299,-462.499999999992));
#34146=CARTESIAN_POINT('Ctrl Pts',(-27.519597245617,46.332430281845,-462.521501238125));
#34147=CARTESIAN_POINT('Ctrl Pts',(-30.6323582333801,62.8326921119377,-440.991469430236));
#34148=CARTESIAN_POINT('Ctrl Pts',(-30.6294184953645,62.8264473376596,-440.999999999994));
#34149=CARTESIAN_POINT('Ctrl Pts',(-23.220257192727,47.0874462155727,-462.499999999992));
#34150=CARTESIAN_POINT('Ctrl Pts',(-23.2128472394025,47.0717055319886,-462.521502298291));
#34151=CARTESIAN_POINT('Ctrl Pts',(-24.9038049544188,63.5523580409965,-440.99146973189));
#34152=CARTESIAN_POINT('Ctrl Pts',(-24.9014153257654,63.5460465225645,-440.999999999994));
#34153=CARTESIAN_POINT('Ctrl Pts',(-18.8785077896217,47.6382644182162,-462.499999999992));
#34154=CARTESIAN_POINT('Ctrl Pts',(-18.8724840252419,47.622354373005,-462.52150305867));
#34155=CARTESIAN_POINT('Ctrl Pts',(-24.8758540410355,63.5558694546237,-440.991469733362));
#34156=CARTESIAN_POINT('Ctrl Pts',(-24.8734670964907,63.5495576105319,-440.999999999994));
#34157=CARTESIAN_POINT('Ctrl Pts',(-18.8573226583922,47.6409520804515,-462.499999999992));
#34158=CARTESIAN_POINT('Ctrl Pts',(-18.8513056577824,47.6250412088575,-462.521503062381));
#34159=CARTESIAN_POINT('Ctrl Pts',(-24.8479031276521,63.5593808682511,-440.991469734834));
#34160=CARTESIAN_POINT('Ctrl Pts',(-24.8455188672159,63.5530686984991,-440.999999999994));
#34161=CARTESIAN_POINT('Ctrl Pts',(-18.8361375271626,47.6436397426871,-462.499999999992));
#34162=CARTESIAN_POINT('Ctrl Pts',(-18.8301272903229,47.6277280447099,-462.521503066091));
#34163=CARTESIAN_POINT('Ctrl Pts',(-24.8199522142688,63.5628922818783,-440.991469736305));
#34164=CARTESIAN_POINT('Ctrl Pts',(-24.8175706379412,63.5565797864666,-440.999999999994));
#34165=CARTESIAN_POINT('Ctrl Pts',(-18.814952395933,47.6463274049225,-462.499999999992));
#34166=CARTESIAN_POINT('Ctrl Pts',(-18.8089489228634,47.6304148805623,-462.521503069801));
#34167=CARTESIAN_POINT('',(-41.9462958339113,60.6491036583583,-440.999972397992));
#34168=CARTESIAN_POINT('Ctrl Pts',(-31.7948796623065,45.4225605594505,-462.499999999992));
#34169=CARTESIAN_POINT('Ctrl Pts',(-32.3589367582276,46.2685042102034,-461.305499732182));
#34170=CARTESIAN_POINT('Ctrl Pts',(-32.9230130678469,47.114453047541,-460.110987971848));
#34171=CARTESIAN_POINT('Ctrl Pts',(-33.4870955758511,47.9604022194252,-458.916474195592));
#34172=CARTESIAN_POINT('Ctrl Pts',(-33.5108390027484,47.9960100109033,-458.866194582021));
#34173=CARTESIAN_POINT('Ctrl Pts',(-33.5345824407334,48.0316178027276,-458.815914965151));
#34174=CARTESIAN_POINT('Ctrl Pts',(-33.5583258888888,48.0672255944517,-458.765635345777));
#34175=CARTESIAN_POINT('Ctrl Pts',(-33.8316335282801,48.4771020974939,-458.186873407305));
#34176=CARTESIAN_POINT('Ctrl Pts',(-34.1049416910635,48.8869789136655,-457.608110953941));
#34177=CARTESIAN_POINT('Ctrl Pts',(-34.3782537048231,49.2968534751887,-457.029350268047));
#34178=CARTESIAN_POINT('Ctrl Pts',(-34.5132877509722,49.4993583694842,-456.743404560452));
#34179=CARTESIAN_POINT('Ctrl Pts',(-34.648322925422,49.7018626398917,-456.457459324899));
#34180=CARTESIAN_POINT('Ctrl Pts',(-34.7833597254613,49.9043659276223,-456.171514872232));
#34181=CARTESIAN_POINT('Ctrl Pts',(-34.9151745034667,50.1020374209471,-455.892393147345));
#34182=CARTESIAN_POINT('Ctrl Pts',(-35.0469908795589,50.2997079600871,-455.613272177396));
#34183=CARTESIAN_POINT('Ctrl Pts',(-35.1788083996884,50.4973775420908,-455.334152087624));
#34184=CARTESIAN_POINT('Ctrl Pts',(-35.348615406454,50.752015013769,-454.974590271215));
#34185=CARTESIAN_POINT('Ctrl Pts',(-35.5184242304502,51.0066509291891,-454.615029897676));
#34186=CARTESIAN_POINT('Ctrl Pts',(-35.6882312710722,51.2612862178012,-454.255470778926));
#34187=CARTESIAN_POINT('Ctrl Pts',(-36.0826190404626,51.8526930470817,-453.420371608195));
#34188=CARTESIAN_POINT('Ctrl Pts',(-36.4769941306178,52.4440976990883,-452.585278532376));
#34189=CARTESIAN_POINT('Ctrl Pts',(-36.87136162915,53.0354928881843,-451.750199183157));
#34190=CARTESIAN_POINT('Ctrl Pts',(-36.8713782411473,53.0355177996066,-451.750164006993));
#34191=CARTESIAN_POINT('Ctrl Pts',(-36.8713948531446,53.035542711029,-451.750128830828));
#34192=CARTESIAN_POINT('Ctrl Pts',(-36.8714114651419,53.0355676224513,-451.750093654664));
#34193=CARTESIAN_POINT('Ctrl Pts',(-37.1088992326438,53.3917052969764,-451.247209588678));
#34194=CARTESIAN_POINT('Ctrl Pts',(-37.3463820495311,53.7478476179124,-450.744321111962));
#34195=CARTESIAN_POINT('Ctrl Pts',(-37.5838553593534,54.1039950517835,-450.241428853719));
#34196=CARTESIAN_POINT('Ctrl Pts',(-37.9100804261045,54.5932467511626,-449.550588857272));
#34197=CARTESIAN_POINT('Ctrl Pts',(-38.2363414682279,55.0824885214636,-448.859751561661));
#34198=CARTESIAN_POINT('Ctrl Pts',(-38.5627017963576,55.5716951867403,-448.168931295036));
#34199=CARTESIAN_POINT('Ctrl Pts',(-38.5630166981229,55.5721672172823,-448.168264729578));
#34200=CARTESIAN_POINT('Ctrl Pts',(-38.5633315999745,55.5726392477937,-448.167598164135));
#34201=CARTESIAN_POINT('Ctrl Pts',(-38.5636465019127,55.5731112782747,-448.166931598707));
#34202=CARTESIAN_POINT('Ctrl Pts',(-38.5760051462592,55.5916365908502,-448.140771565806));
#34203=CARTESIAN_POINT('Ctrl Pts',(-38.5883639239044,55.6101618563835,-448.11461155567));
#34204=CARTESIAN_POINT('Ctrl Pts',(-38.6007228216993,55.6286870798238,-448.088451565684));
#34205=CARTESIAN_POINT('Ctrl Pts',(-38.6160934753,55.6517267389508,-448.055916613866));
#34206=CARTESIAN_POINT('Ctrl Pts',(-38.6314643147417,55.6747663329655,-448.023381693218));
#34207=CARTESIAN_POINT('Ctrl Pts',(-38.6468353147218,55.6978058713775,-447.990846798726));
#34208=CARTESIAN_POINT('Ctrl Pts',(-38.8979459656751,56.0741947527639,-447.459335605872));
#34209=CARTESIAN_POINT('Ctrl Pts',(-39.1490995352716,56.4505687718856,-446.927831437525));
#34210=CARTESIAN_POINT('Ctrl Pts',(-39.4001855850623,56.8269694640148,-446.396312247445));
#34211=CARTESIAN_POINT('Ctrl Pts',(-39.4034915843839,56.8319254559302,-446.389313841586));
#34212=CARTESIAN_POINT('Ctrl Pts',(-39.4072720742608,56.8375927809872,-446.381310960185));
#34213=CARTESIAN_POINT('Ctrl Pts',(-39.4101046309297,56.841837216879,-446.375317027575));
#34214=CARTESIAN_POINT('Ctrl Pts',(-39.5913882577387,57.1134811139516,-445.99170534054));
#34215=CARTESIAN_POINT('Ctrl Pts',(-39.7877372632166,57.4079275655785,-445.575932518066));
#34216=CARTESIAN_POINT('Ctrl Pts',(-39.9991450289739,57.7251779818922,-445.127998595665));
#34217=CARTESIAN_POINT('Ctrl Pts',(-40.0793695533942,57.8455674277563,-444.958017678609));
#34218=CARTESIAN_POINT('Ctrl Pts',(-40.1617685171492,57.9692393496446,-444.78340557784));
#34219=CARTESIAN_POINT('Ctrl Pts',(-40.2463321871013,58.0961960812351,-444.604161989806));
#34220=CARTESIAN_POINT('Ctrl Pts',(-40.2490197084776,58.1002308981986,-444.598465442166));
#34221=CARTESIAN_POINT('Ctrl Pts',(-40.2517094161308,58.1042690329628,-444.592764216566));
#34222=CARTESIAN_POINT('Ctrl Pts',(-40.2544013097201,58.108310485609,-444.587058312992));
#34223=CARTESIAN_POINT('Ctrl Pts',(-40.2547914092775,58.1088961584213,-444.586231433925));
#34224=CARTESIAN_POINT('Ctrl Pts',(-40.2551815547414,58.1094819009116,-444.585404456617));
#34225=CARTESIAN_POINT('Ctrl Pts',(-40.2555717461105,58.1100677130802,-444.584577381068));
#34226=CARTESIAN_POINT('Ctrl Pts',(-40.2557149406528,58.1102826976032,-444.584273856402));
#34227=CARTESIAN_POINT('Ctrl Pts',(-40.2558581413776,58.1104976915104,-444.583970318506));
#34228=CARTESIAN_POINT('Ctrl Pts',(-40.2560013482848,58.1107126948018,-444.583666767379));
#34229=CARTESIAN_POINT('Ctrl Pts',(-40.2796849784717,58.1462700470485,-444.533465329607));
#34230=CARTESIAN_POINT('Ctrl Pts',(-40.303537699453,58.1820840635307,-444.482902015482));
#34231=CARTESIAN_POINT('Ctrl Pts',(-40.3275595667118,58.2181546889882,-444.431976878569));
#34232=CARTESIAN_POINT('Ctrl Pts',(-40.4124840726278,58.3456751690598,-444.251941245018));
#34233=CARTESIAN_POINT('Ctrl Pts',(-40.499520101303,58.4764037568062,-444.067382958364));
#34234=CARTESIAN_POINT('Ctrl Pts',(-40.5886753472471,58.6103388069207,-443.878302012751));
#34235=CARTESIAN_POINT('Ctrl Pts',(-40.6165363616047,58.6521935100814,-443.819214217247));
#34236=CARTESIAN_POINT('Ctrl Pts',(-40.6446043519804,58.6943613397393,-443.759684755887));
#34237=CARTESIAN_POINT('Ctrl Pts',(-40.6728796563084,58.7368422234442,-443.699713628641));
#34238=CARTESIAN_POINT('Ctrl Pts',(-40.6747646765969,58.7396742823579,-443.695715553492));
#34239=CARTESIAN_POINT('Ctrl Pts',(-40.6760795623318,58.7416497712972,-443.692926715857));
#34240=CARTESIAN_POINT('Ctrl Pts',(-40.678537478369,58.7453425748796,-443.687713514316));
#34241=CARTESIAN_POINT('Ctrl Pts',(-40.8368925478841,58.9832571981406,-443.351844884157));
#34242=CARTESIAN_POINT('Ctrl Pts',(-40.9821297055412,59.2015062105175,-443.043746120084));
#34243=CARTESIAN_POINT('Ctrl Pts',(-41.114288823774,59.400066662282,-442.763435022771));
#34244=CARTESIAN_POINT('Ctrl Pts',(-41.2700380822643,59.6340697605274,-442.433088951029));
#34245=CARTESIAN_POINT('Ctrl Pts',(-41.4076231632199,59.8407285235985,-442.141335825954));
#34246=CARTESIAN_POINT('Ctrl Pts',(-41.5270507342642,60.0200390015437,-441.888178771391));
#34247=CARTESIAN_POINT('Ctrl Pts',(-41.6954461091794,60.2728705286002,-441.531222025617));
#34248=CARTESIAN_POINT('Ctrl Pts',(-41.8277387540249,60.4713302688281,-441.250999947206));
#34249=CARTESIAN_POINT('Ctrl Pts',(-41.9238600911249,60.6154630592316,-441.047475323372));
#34250=CARTESIAN_POINT('Ctrl Pts',(-41.929943127075,60.6245844985714,-441.034595273626));
#34251=CARTESIAN_POINT('Ctrl Pts',(-41.9358812893885,60.6334883672191,-441.022022388381));
#34252=CARTESIAN_POINT('Ctrl Pts',(-41.9416745594323,60.6421746787551,-441.009756655798));
#34253=CARTESIAN_POINT('Ctrl Pts',(-41.94322536715,60.6444999283752,-441.006473226472));
#34254=CARTESIAN_POINT('Ctrl Pts',(-41.9447657920937,60.6468095881562,-441.003211807279));
#34255=CARTESIAN_POINT('Ctrl Pts',(-41.9462958339113,60.6491036583582,-440.999972397991));
#34256=CARTESIAN_POINT('Ctrl Pts',(-33.4829940317438,62.2764393483424,-440.999971988125));
#34257=CARTESIAN_POINT('Ctrl Pts',(-35.2473688614902,61.9765046694296,-440.999378147116));
#34258=CARTESIAN_POINT('Ctrl Pts',(-37.0072017317725,61.652949072738,-440.998941663519));
#34259=CARTESIAN_POINT('Ctrl Pts',(-38.7624945086218,61.3057812102067,-440.999059709867));
#34260=CARTESIAN_POINT('Ctrl Pts',(-39.8254271432111,61.0955507257929,-440.999131193848));
#34261=CARTESIAN_POINT('Ctrl Pts',(-40.8866947611648,60.876660597413,-440.999406024634));
#34262=CARTESIAN_POINT('Ctrl Pts',(-41.9462958339112,60.6491036583585,-440.999972397992));
#34263=CARTESIAN_POINT('Ctrl Pts',(-38.7647784196973,41.8087166343715,-462.499999999991));
#34264=CARTESIAN_POINT('Ctrl Pts',(-39.7995127746359,42.4001734346326,-461.308933337928));
#34265=CARTESIAN_POINT('Ctrl Pts',(-40.8357048397936,42.9924662438129,-460.119580355696));
#34266=CARTESIAN_POINT('Ctrl Pts',(-41.8710255300635,43.5843887879793,-458.928944911376));
#34267=CARTESIAN_POINT('Ctrl Pts',(-41.9145943466774,43.6092983305189,-458.878840071576));
#34268=CARTESIAN_POINT('Ctrl Pts',(-41.9581616507534,43.6342072350156,-458.828732976872));
#34269=CARTESIAN_POINT('Ctrl Pts',(-42.0017269585341,43.6591152324882,-458.778623239637));
#34270=CARTESIAN_POINT('Ctrl Pts',(-42.5030969739151,43.9457681614373,-458.201936857561));
#34271=CARTESIAN_POINT('Ctrl Pts',(-43.0041933315388,44.2322956141741,-457.624895577444));
#34272=CARTESIAN_POINT('Ctrl Pts',(-43.5042383164771,44.5182643009072,-457.046887196222));
#34273=CARTESIAN_POINT('Ctrl Pts',(-43.7512069378789,44.659502178406,-456.761413014161));
#34274=CARTESIAN_POINT('Ctrl Pts',(-43.9936639707697,44.8077097666099,-456.475636259694));
#34275=CARTESIAN_POINT('Ctrl Pts',(-44.2358141697137,44.9557921216003,-456.189595586012));
#34276=CARTESIAN_POINT('Ctrl Pts',(-44.4721203184572,45.1003006586869,-455.910458214757));
#34277=CARTESIAN_POINT('Ctrl Pts',(-44.7070275434294,45.2465058687078,-455.631041156453));
#34278=CARTESIAN_POINT('Ctrl Pts',(-44.9403037377182,45.3946741562122,-455.351299568589));
#34279=CARTESIAN_POINT('Ctrl Pts',(-45.240700079509,45.5854746434694,-454.991068427573));
#34280=CARTESIAN_POINT('Ctrl Pts',(-45.5381389695975,45.7798299821193,-454.630250129497));
#34281=CARTESIAN_POINT('Ctrl Pts',(-45.8336313302898,45.9765136570778,-454.269041480137));
#34282=CARTESIAN_POINT('Ctrl Pts',(-46.5193665414722,46.4329482026873,-453.430801571433));
#34283=CARTESIAN_POINT('Ctrl Pts',(-47.1964439938651,46.8997279795032,-452.59080707252));
#34284=CARTESIAN_POINT('Ctrl Pts',(-47.879046287083,47.3598643087836,-451.751944466043));
#34285=CARTESIAN_POINT('Ctrl Pts',(-48.2897059737973,47.6366864681957,-451.247277167684));
#34286=CARTESIAN_POINT('Ctrl Pts',(-48.7024673284649,47.910980788196,-450.743045916156));
#34287=CARTESIAN_POINT('Ctrl Pts',(-49.1164444213912,48.1838184566469,-450.239075976318));
#34288=CARTESIAN_POINT('Ctrl Pts',(-49.6846286879767,48.5582886222539,-449.547376373752));
#34289=CARTESIAN_POINT('Ctrl Pts',(-50.254528115132,48.9307093367966,-448.856042300473));
#34290=CARTESIAN_POINT('Ctrl Pts',(-50.8246359664257,49.3028643087629,-448.164779253762));
#34291=CARTESIAN_POINT('Ctrl Pts',(-50.825185828888,49.3032232479509,-448.164112538508));
#34292=CARTESIAN_POINT('Ctrl Pts',(-50.8257356894882,49.3035821893701,-448.163445822851));
#34293=CARTESIAN_POINT('Ctrl Pts',(-50.8262855481909,49.3039411330631,-448.162779106782));
#34294=CARTESIAN_POINT('Ctrl Pts',(-50.8478649914022,49.3180280339392,-448.13661354557));
#34295=CARTESIAN_POINT('Ctrl Pts',(-50.8694413893419,49.332118585145,-448.110447322959));
#34296=CARTESIAN_POINT('Ctrl Pts',(-50.8910131109905,49.3462147596686,-448.084280059973));
#34297=CARTESIAN_POINT('Ctrl Pts',(-50.9178408197646,49.3637454913882,-448.051737098301));
#34298=CARTESIAN_POINT('Ctrl Pts',(-50.9446603430864,49.3812860730376,-448.019192307034));
#34299=CARTESIAN_POINT('Ctrl Pts',(-50.971478129671,49.3988287152465,-447.986647158958));
#34300=CARTESIAN_POINT('Ctrl Pts',(-51.9014817827599,50.0071832223397,-446.858026550983));
#34301=CARTESIAN_POINT('Ctrl Pts',(-52.830781565206,50.6163348829018,-445.72929845917));
#34302=CARTESIAN_POINT('Ctrl Pts',(-53.7602372678272,51.2252767470049,-444.600618965139));
#34303=CARTESIAN_POINT('Ctrl Pts',(-53.7649288881994,51.2283505073219,-444.594921721373));
#34304=CARTESIAN_POINT('Ctrl Pts',(-53.7696205154581,51.2314242588856,-444.589224479561));
#34305=CARTESIAN_POINT('Ctrl Pts',(-53.7743121497644,51.2344980015086,-444.583527239736));
#34306=CARTESIAN_POINT('Ctrl Pts',(-53.7749926814309,51.2349438545,-444.582700842822));
#34307=CARTESIAN_POINT('Ctrl Pts',(-53.7756732132458,51.2353897073031,-444.581874445952));
#34308=CARTESIAN_POINT('Ctrl Pts',(-53.7766035309538,51.2359992078201,-444.580744724428));
#34309=CARTESIAN_POINT('Ctrl Pts',(-53.7768533167191,51.2361628556965,-444.580441399742));
#34310=CARTESIAN_POINT('Ctrl Pts',(-54.7572059250983,51.8784435905557,-443.38996075712));
#34311=CARTESIAN_POINT('Ctrl Pts',(-55.7376166746149,52.5201719518042,-442.199871278583));
#34312=CARTESIAN_POINT('Ctrl Pts',(-56.7204946137808,53.1638621099781,-441.006502807678));
#34313=CARTESIAN_POINT('Ctrl Pts',(-56.7231781091608,53.1656195429638,-441.003244619903));
#34314=CARTESIAN_POINT('Ctrl Pts',(-56.7850035851904,53.206109380605,-440.928178664855));
#34315=CARTESIAN_POINT('Ctrl Pts',(-56.8441455674789,53.2448417837246,-440.856370897749));
#34316=CARTESIAN_POINT('Ctrl Pts',(-56.9032875497673,53.2835741868442,-440.784563130644));
#34317=CARTESIAN_POINT('Ctrl Pts',(-38.7453917572008,41.8263434012394,-462.499999999991));
#34318=CARTESIAN_POINT('Ctrl Pts',(-39.7788308189521,42.4190348163309,-461.308907091454));
#34319=CARTESIAN_POINT('Ctrl Pts',(-40.8137298218099,43.0125653951676,-460.119519192124));
#34320=CARTESIAN_POINT('Ctrl Pts',(-41.8477747406438,43.6056914173716,-458.928850923932));
#34321=CARTESIAN_POINT('Ctrl Pts',(-41.8912898696879,43.6306516051987,-458.878744702824));
#34322=CARTESIAN_POINT('Ctrl Pts',(-41.9348035168151,43.6556110942547,-458.828636230518));
#34323=CARTESIAN_POINT('Ctrl Pts',(-41.9783151993904,43.6805696127678,-458.778525120191));
#34324=CARTESIAN_POINT('Ctrl Pts',(-42.4790680707299,43.96780396157,-458.201822935923));
#34325=CARTESIAN_POINT('Ctrl Pts',(-42.9795514885468,44.2549044214201,-457.624766450826));
#34326=CARTESIAN_POINT('Ctrl Pts',(-43.4789894486357,44.5414334488357,-457.046744684544));
#34327=CARTESIAN_POINT('Ctrl Pts',(-43.7256582648306,44.6829480745672,-456.761263891698));
#34328=CARTESIAN_POINT('Ctrl Pts',(-43.9678169353505,44.8314293212802,-456.47548097038));
#34329=CARTESIAN_POINT('Ctrl Pts',(-44.2096704208597,44.9797817325908,-456.189434721086));
#34330=CARTESIAN_POINT('Ctrl Pts',(-44.4456870170472,45.1245538084617,-455.910291908782));
#34331=CARTESIAN_POINT('Ctrl Pts',(-44.680306259769,45.2710191268505,-455.630869972474));
#34332=CARTESIAN_POINT('Ctrl Pts',(-44.913296233648,45.4194436160569,-455.351124206549));
#34333=CARTESIAN_POINT('Ctrl Pts',(-45.2133240013361,45.6105740214795,-454.990887685325));
#34334=CARTESIAN_POINT('Ctrl Pts',(-45.5103972388836,45.8052528000895,-454.630065167715));
#34335=CARTESIAN_POINT('Ctrl Pts',(-45.8055272775946,46.0022524198349,-454.268853751822));
#34336=CARTESIAN_POINT('Ctrl Pts',(-46.4904216652111,46.4594201636385,-453.430607422953));
#34337=CARTESIAN_POINT('Ctrl Pts',(-47.1666762305336,46.9268927739179,-452.5906143289));
#34338=CARTESIAN_POINT('Ctrl Pts',(-47.8484786847142,47.3876688621575,-451.751764605686));
#34339=CARTESIAN_POINT('Ctrl Pts',(-48.2586571810607,47.6648759063206,-451.247105058015));
#34340=CARTESIAN_POINT('Ctrl Pts',(-48.6709293769293,47.9395596801869,-450.742882074723));
#34341=CARTESIAN_POINT('Ctrl Pts',(-49.0844109446666,48.2127905597223,-450.238920749702));
#34342=CARTESIAN_POINT('Ctrl Pts',(-49.6519151020844,48.587800408214,-449.547232970989));
#34343=CARTESIAN_POINT('Ctrl Pts',(-50.2211224273152,48.9607678833433,-448.855911374438));
#34344=CARTESIAN_POINT('Ctrl Pts',(-50.7905303259489,49.3334745944688,-448.164661015305));
#34345=CARTESIAN_POINT('Ctrl Pts',(-50.7910795133149,49.3338340658028,-448.163994312287));
#34346=CARTESIAN_POINT('Ctrl Pts',(-50.7916286988116,49.3341935393728,-448.163327608868));
#34347=CARTESIAN_POINT('Ctrl Pts',(-50.7921778824033,49.3345530152211,-448.162660905037));
#34348=CARTESIAN_POINT('Ctrl Pts',(-50.8137308305952,49.348660800764,-448.136495824087));
#34349=CARTESIAN_POINT('Ctrl Pts',(-50.8352807222728,49.3627722437666,-448.11033008204));
#34350=CARTESIAN_POINT('Ctrl Pts',(-50.8568259266415,49.3768893171035,-448.084163299895));
#34351=CARTESIAN_POINT('Ctrl Pts',(-50.8836206571549,49.3944460396681,-448.051620936223));
#34352=CARTESIAN_POINT('Ctrl Pts',(-50.910407185175,49.4120126230145,-448.019076743385));
#34353=CARTESIAN_POINT('Ctrl Pts',(-50.937191959849,49.4295812775534,-447.986532194121));
#34354=CARTESIAN_POINT('Ctrl Pts',(-51.8660508056535,50.0388378561823,-446.857932352111));
#34355=CARTESIAN_POINT('Ctrl Pts',(-52.7941858068855,50.6489043755752,-445.729225486989));
#34356=CARTESIAN_POINT('Ctrl Pts',(-53.7224747742633,51.2587647535248,-444.600565757327));
#34357=CARTESIAN_POINT('Ctrl Pts',(-53.7271605052976,51.261843150231,-444.594868613325));
#34358=CARTESIAN_POINT('Ctrl Pts',(-53.7318462431683,51.2649215382768,-444.589171471241));
#34359=CARTESIAN_POINT('Ctrl Pts',(-53.7365319880393,51.267999917474,-444.583474331106));
#34360=CARTESIAN_POINT('Ctrl Pts',(-53.7372116654306,51.2684464430104,-444.582647948653));
#34361=CARTESIAN_POINT('Ctrl Pts',(-53.7378913429692,51.2688929683606,-444.581821566241));
#34362=CARTESIAN_POINT('Ctrl Pts',(-53.7388204928419,51.2695033882821,-444.580691864483));
#34363=CARTESIAN_POINT('Ctrl Pts',(-53.7390699650489,51.2696672830144,-444.580388545105));
#34364=CARTESIAN_POINT('Ctrl Pts',(-54.7181919280243,51.9129168722811,-443.389928730339));
#34365=CARTESIAN_POINT('Ctrl Pts',(-55.6973702941219,52.5556178438312,-442.199858435399));
#34366=CARTESIAN_POINT('Ctrl Pts',(-56.679031605489,53.2002765515568,-441.006505296162));
#34367=CARTESIAN_POINT('Ctrl Pts',(-56.6817117793207,53.2020366288693,-441.003247150217));
#34368=CARTESIAN_POINT('Ctrl Pts',(-56.7434607329299,53.2425873884486,-440.928182158226));
#34369=CARTESIAN_POINT('Ctrl Pts',(-56.8025295142029,53.28137806923,-440.856375312376));
#34370=CARTESIAN_POINT('Ctrl Pts',(-56.8615982954759,53.3201687500114,-440.784568466526));
#34371=CARTESIAN_POINT('Ctrl Pts',(-38.7260050947043,41.8439701681072,-462.499999999991));
#34372=CARTESIAN_POINT('Ctrl Pts',(-39.7581488632683,42.4378961980291,-461.30888084498));
#34373=CARTESIAN_POINT('Ctrl Pts',(-40.7917548038261,43.0326645465224,-460.119458028552));
#34374=CARTESIAN_POINT('Ctrl Pts',(-41.8245239512239,43.626994046764,-458.928756936488));
#34375=CARTESIAN_POINT('Ctrl Pts',(-41.8679853926983,43.6520048798785,-458.878649334071));
#34376=CARTESIAN_POINT('Ctrl Pts',(-41.9114453828767,43.6770149534938,-458.828539484164));
#34377=CARTESIAN_POINT('Ctrl Pts',(-41.9549034402465,43.7020239930474,-458.778427000744));
#34378=CARTESIAN_POINT('Ctrl Pts',(-42.4550391675447,43.9898397617028,-458.201709014284));
#34379=CARTESIAN_POINT('Ctrl Pts',(-42.9549096455548,44.2775132286661,-457.624637324207));
#34380=CARTESIAN_POINT('Ctrl Pts',(-43.4537405807944,44.5646025967642,-457.046602172866));
#34381=CARTESIAN_POINT('Ctrl Pts',(-43.7001095917822,44.7063939707285,-456.761114769235));
#34382=CARTESIAN_POINT('Ctrl Pts',(-43.9419698999314,44.8551488759503,-456.475325681066));
#34383=CARTESIAN_POINT('Ctrl Pts',(-44.1835266720058,45.0037713435814,-456.18927385616));
#34384=CARTESIAN_POINT('Ctrl Pts',(-44.4192537156373,45.1488069582364,-455.910125602806));
#34385=CARTESIAN_POINT('Ctrl Pts',(-44.6535849761086,45.2955323849931,-455.630698788494));
#34386=CARTESIAN_POINT('Ctrl Pts',(-44.886288729578,45.4442130759016,-455.350948844508));
#34387=CARTESIAN_POINT('Ctrl Pts',(-45.1859479231632,45.6356733994895,-454.990706943076));
#34388=CARTESIAN_POINT('Ctrl Pts',(-45.4826555081698,45.8306756180597,-454.629880205933));
#34389=CARTESIAN_POINT('Ctrl Pts',(-45.7774232248994,46.0279911825921,-454.268666023506));
#34390=CARTESIAN_POINT('Ctrl Pts',(-46.46147678895,46.4858921245897,-453.430413274473));
#34391=CARTESIAN_POINT('Ctrl Pts',(-47.1369084672023,46.9540575683327,-452.590421585279));
#34392=CARTESIAN_POINT('Ctrl Pts',(-47.8179110823453,47.4154734155314,-451.75158474533));
#34393=CARTESIAN_POINT('Ctrl Pts',(-48.227608388324,47.6930653444455,-451.246932948346));
#34394=CARTESIAN_POINT('Ctrl Pts',(-48.6393914253937,47.9681385721777,-450.74271823329));
#34395=CARTESIAN_POINT('Ctrl Pts',(-49.052377467942,48.2417626627977,-450.238765523087));
#34396=CARTESIAN_POINT('Ctrl Pts',(-49.6192015161921,48.6173121941742,-449.547089568225));
#34397=CARTESIAN_POINT('Ctrl Pts',(-50.1877167394984,48.9908264298899,-448.855780448404));
#34398=CARTESIAN_POINT('Ctrl Pts',(-50.7564246854722,49.3640848801747,-448.164542776848));
#34399=CARTESIAN_POINT('Ctrl Pts',(-50.7569731977418,49.3644448836548,-448.163876086068));
#34400=CARTESIAN_POINT('Ctrl Pts',(-50.7575217081349,49.3648048893754,-448.163209394885));
#34401=CARTESIAN_POINT('Ctrl Pts',(-50.7580702166158,49.3651648973791,-448.162542703291));
#34402=CARTESIAN_POINT('Ctrl Pts',(-50.7795966697881,49.3792935675887,-448.136378102604));
#34403=CARTESIAN_POINT('Ctrl Pts',(-50.8011200552037,49.3934259023882,-448.110212841121));
#34404=CARTESIAN_POINT('Ctrl Pts',(-50.8226387422926,49.4075638745383,-448.084046539819));
#34405=CARTESIAN_POINT('Ctrl Pts',(-50.8494004945451,49.425146587948,-448.051504774145));
#34406=CARTESIAN_POINT('Ctrl Pts',(-50.8761540272635,49.4427391729914,-448.018961179735));
#34407=CARTESIAN_POINT('Ctrl Pts',(-50.902905790027,49.4603338398603,-447.986417229284));
#34408=CARTESIAN_POINT('Ctrl Pts',(-51.8306198285471,50.0704924900249,-446.857838153238));
#34409=CARTESIAN_POINT('Ctrl Pts',(-52.757590048565,50.6814738682486,-445.729152514807));
#34410=CARTESIAN_POINT('Ctrl Pts',(-53.6847122806995,51.2922527600448,-444.600512549515));
#34411=CARTESIAN_POINT('Ctrl Pts',(-53.6893921223957,51.29533579314,-444.594815505278));
#34412=CARTESIAN_POINT('Ctrl Pts',(-53.6940719708786,51.2984188176681,-444.589118462921));
#34413=CARTESIAN_POINT('Ctrl Pts',(-53.6987518263143,51.3015018334394,-444.583421422477));
#34414=CARTESIAN_POINT('Ctrl Pts',(-53.6994306494303,51.3019490315209,-444.582595054483));
#34415=CARTESIAN_POINT('Ctrl Pts',(-53.7001094726926,51.3023962294181,-444.581768686531));
#34416=CARTESIAN_POINT('Ctrl Pts',(-53.70103745473,51.3030075687442,-444.580639004539));
#34417=CARTESIAN_POINT('Ctrl Pts',(-53.7012866133788,51.3031717103323,-444.580335690467));
#34418=CARTESIAN_POINT('Ctrl Pts',(-54.6791779309502,51.9473901540065,-443.389896703558));
#34419=CARTESIAN_POINT('Ctrl Pts',(-55.6571239136289,52.5910637358582,-442.199845592215));
#34420=CARTESIAN_POINT('Ctrl Pts',(-56.6375685971972,53.2366909931355,-441.006507784646));
#34421=CARTESIAN_POINT('Ctrl Pts',(-56.6402454494806,53.2384537147748,-441.003249680531));
#34422=CARTESIAN_POINT('Ctrl Pts',(-56.7019178806694,53.2790653962921,-440.928185651597));
#34423=CARTESIAN_POINT('Ctrl Pts',(-56.7609134609269,53.3179143547354,-440.856379727003));
#34424=CARTESIAN_POINT('Ctrl Pts',(-56.8199090411844,53.3567633131786,-440.78457380241));
#34425=CARTESIAN_POINT('Ctrl Pts',(-38.7066184322078,41.8615969349749,-462.499999999991));
#34426=CARTESIAN_POINT('Ctrl Pts',(-39.7374669075845,42.4567575797274,-461.308854598505));
#34427=CARTESIAN_POINT('Ctrl Pts',(-40.7697797858423,43.0527636978772,-460.11939686498));
#34428=CARTESIAN_POINT('Ctrl Pts',(-41.8012731618041,43.6482966761564,-458.928662949044));
#34429=CARTESIAN_POINT('Ctrl Pts',(-41.8446809157088,43.6733581545582,-458.878553965319));
#34430=CARTESIAN_POINT('Ctrl Pts',(-41.8880872489384,43.6984188127329,-458.82844273781));
#34431=CARTESIAN_POINT('Ctrl Pts',(-41.9314916811027,43.723478373327,-458.778328881298));
#34432=CARTESIAN_POINT('Ctrl Pts',(-42.4310102643594,44.0118755618356,-458.201595092646));
#34433=CARTESIAN_POINT('Ctrl Pts',(-42.9302678025629,44.300122035912,-457.624508197589));
#34434=CARTESIAN_POINT('Ctrl Pts',(-43.428491712953,44.5877717446927,-457.046459661188));
#34435=CARTESIAN_POINT('Ctrl Pts',(-43.6745609187339,44.7298398668897,-456.760965646773));
#34436=CARTESIAN_POINT('Ctrl Pts',(-43.9161228645122,44.8788684306205,-456.475170391752));
#34437=CARTESIAN_POINT('Ctrl Pts',(-44.1573829231518,45.027760954572,-456.189112991235));
#34438=CARTESIAN_POINT('Ctrl Pts',(-44.3928204142273,45.1730601080112,-455.909959296831));
#34439=CARTESIAN_POINT('Ctrl Pts',(-44.6268636924482,45.3200456431357,-455.630527604515));
#34440=CARTESIAN_POINT('Ctrl Pts',(-44.8592812255079,45.4689825357462,-455.350773482467));
#34441=CARTESIAN_POINT('Ctrl Pts',(-45.1585718449904,45.6607727774995,-454.990526200827));
#34442=CARTESIAN_POINT('Ctrl Pts',(-45.454913777456,45.8560984360299,-454.629695244152));
#34443=CARTESIAN_POINT('Ctrl Pts',(-45.7493191722042,46.0537299453492,-454.268478295191));
#34444=CARTESIAN_POINT('Ctrl Pts',(-46.432531912689,46.5123640855408,-453.430219125993));
#34445=CARTESIAN_POINT('Ctrl Pts',(-47.1071407038709,46.9812223627475,-452.590228841659));
#34446=CARTESIAN_POINT('Ctrl Pts',(-47.7873434799765,47.4432779689052,-451.751404884973));
#34447=CARTESIAN_POINT('Ctrl Pts',(-48.1965595955874,47.7212547825704,-451.246760838677));
#34448=CARTESIAN_POINT('Ctrl Pts',(-48.6078534738581,47.9967174641686,-450.742554391857));
#34449=CARTESIAN_POINT('Ctrl Pts',(-49.0203439912174,48.2707347658732,-450.238610296471));
#34450=CARTESIAN_POINT('Ctrl Pts',(-49.5864879302998,48.6468239801343,-449.546946165461));
#34451=CARTESIAN_POINT('Ctrl Pts',(-50.1543110516816,49.0208849764366,-448.855649522369));
#34452=CARTESIAN_POINT('Ctrl Pts',(-50.7223190449954,49.3946951658807,-448.16442453839));
#34453=CARTESIAN_POINT('Ctrl Pts',(-50.7228668821688,49.3950557015069,-448.163757859847));
#34454=CARTESIAN_POINT('Ctrl Pts',(-50.7234147174583,49.3954162393782,-448.163091180901));
#34455=CARTESIAN_POINT('Ctrl Pts',(-50.7239625508283,49.3957767795372,-448.162424501545));
#34456=CARTESIAN_POINT('Ctrl Pts',(-50.745462508981,49.4099263344135,-448.136260381121));
#34457=CARTESIAN_POINT('Ctrl Pts',(-50.7669593881346,49.4240795610099,-448.110095600202));
#34458=CARTESIAN_POINT('Ctrl Pts',(-50.7884515579436,49.4382384319732,-448.083929779741));
#34459=CARTESIAN_POINT('Ctrl Pts',(-50.8151803319354,49.4558471362279,-448.051388612068));
#34460=CARTESIAN_POINT('Ctrl Pts',(-50.8419008693521,49.4734657229684,-448.018845616087));
#34461=CARTESIAN_POINT('Ctrl Pts',(-50.868619620205,49.4910864021673,-447.986302264447));
#34462=CARTESIAN_POINT('Ctrl Pts',(-51.7951888514407,50.1021471238675,-446.857743954364));
#34463=CARTESIAN_POINT('Ctrl Pts',(-52.7209942902445,50.714043360922,-445.729079542625));
#34464=CARTESIAN_POINT('Ctrl Pts',(-53.6469497871357,51.3257407665647,-444.600459341703));
#34465=CARTESIAN_POINT('Ctrl Pts',(-53.6516237394938,51.328828436049,-444.594762397231));
#34466=CARTESIAN_POINT('Ctrl Pts',(-53.6562976985889,51.3319160970593,-444.589065454601));
#34467=CARTESIAN_POINT('Ctrl Pts',(-53.6609716645893,51.3350037494048,-444.583368513846));
#34468=CARTESIAN_POINT('Ctrl Pts',(-53.66164963343,51.3354516200314,-444.582542160313));
#34469=CARTESIAN_POINT('Ctrl Pts',(-53.662327602416,51.3358994904756,-444.581715806821));
#34470=CARTESIAN_POINT('Ctrl Pts',(-53.663254416618,51.3365117492062,-444.580586144595));
#34471=CARTESIAN_POINT('Ctrl Pts',(-53.6635032617087,51.3366761376502,-444.58028283583));
#34472=CARTESIAN_POINT('Ctrl Pts',(-54.6401639338761,51.9818634357318,-443.389864676778));
#34473=CARTESIAN_POINT('Ctrl Pts',(-55.6168775331359,52.6265096278852,-442.199832749031));
#34474=CARTESIAN_POINT('Ctrl Pts',(-56.5961055889053,53.2731054347143,-441.00651027313));
#34475=CARTESIAN_POINT('Ctrl Pts',(-56.5987791196405,53.2748708006803,-441.003252210846));
#34476=CARTESIAN_POINT('Ctrl Pts',(-56.660375028409,53.3155434041358,-440.928189144968));
#34477=CARTESIAN_POINT('Ctrl Pts',(-56.7192974076509,53.3544506402408,-440.85638414163));
#34478=CARTESIAN_POINT('Ctrl Pts',(-56.7782197868929,53.3933578763459,-440.784579138293));
#34479=CARTESIAN_POINT('Ctrl Pts',(-38.3840553815676,42.1548781377002,-462.499999999991));
#34480=CARTESIAN_POINT('Ctrl Pts',(-39.3933522504188,42.7705807981887,-461.308417899162));
#34481=CARTESIAN_POINT('Ctrl Pts',(-40.4041506405478,43.3871814233334,-460.118379200986));
#34482=CARTESIAN_POINT('Ctrl Pts',(-41.4144172206949,44.0027383509268,-458.927099148328));
#34483=CARTESIAN_POINT('Ctrl Pts',(-41.4569316993248,44.0286424858926,-458.876967181839));
#34484=CARTESIAN_POINT('Ctrl Pts',(-41.4994452667629,44.0545447902129,-458.826833033245));
#34485=CARTESIAN_POINT('Ctrl Pts',(-41.5419574612932,44.0804449401011,-458.776696330672));
#34486=CARTESIAN_POINT('Ctrl Pts',(-42.031207754961,44.378516024855,-458.199699618824));
#34487=CARTESIAN_POINT('Ctrl Pts',(-42.5202669553144,44.6762964206426,-457.622359737223));
#34488=CARTESIAN_POINT('Ctrl Pts',(-43.0083909432826,44.9732693019898,-457.044088494844));
#34489=CARTESIAN_POINT('Ctrl Pts',(-43.2494718700247,45.1199420720588,-456.758484487548));
#34490=CARTESIAN_POINT('Ctrl Pts',(-43.48606954325,45.2735238756008,-456.472586625987));
#34491=CARTESIAN_POINT('Ctrl Pts',(-43.7223927649944,45.4269097047084,-456.186436456212));
#34492=CARTESIAN_POINT('Ctrl Pts',(-43.9530125647411,45.5765937219271,-455.907192231443));
#34493=CARTESIAN_POINT('Ctrl Pts',(-44.1822642790075,45.7279070441918,-455.627679376945));
#34494=CARTESIAN_POINT('Ctrl Pts',(-44.4099195623238,45.8811067232721,-455.347855738637));
#34495=CARTESIAN_POINT('Ctrl Pts',(-44.7030776983524,46.0783862755194,-454.987518938944));
#34496=CARTESIAN_POINT('Ctrl Pts',(-44.9933357574793,46.2790934575717,-454.626617775994));
#34497=CARTESIAN_POINT('Ctrl Pts',(-45.2817126940726,46.4819817827217,-454.265354796337));
#34498=CARTESIAN_POINT('Ctrl Pts',(-45.9509354755063,46.9528151679476,-453.426988805868));
#34499=CARTESIAN_POINT('Ctrl Pts',(-46.6118527422302,47.4332010856463,-452.58702189615));
#34500=CARTESIAN_POINT('Ctrl Pts',(-47.2787474762744,47.9059012574457,-451.748412296366));
#34501=CARTESIAN_POINT('Ctrl Pts',(-47.6799573539367,48.1902819376597,-451.243897209111));
#34502=CARTESIAN_POINT('Ctrl Pts',(-48.0831124123112,48.4722245085679,-450.739828332511));
#34503=CARTESIAN_POINT('Ctrl Pts',(-48.4873581832285,48.7527842136913,-450.236027573909));
#34504=CARTESIAN_POINT('Ctrl Pts',(-49.0421861937476,49.1378528878107,-449.54456017288));
#34505=CARTESIAN_POINT('Ctrl Pts',(-49.598493846277,49.521011105607,-448.853471122598));
#34506=CARTESIAN_POINT('Ctrl Pts',(-50.15485574706,49.9040013520307,-448.162457239611));
#34507=CARTESIAN_POINT('Ctrl Pts',(-50.1553923517111,49.9043707417163,-448.161790764672));
#34508=CARTESIAN_POINT('Ctrl Pts',(-50.1559289543568,49.9047401337239,-448.161124289334));
#34509=CARTESIAN_POINT('Ctrl Pts',(-50.1564655549617,49.9051095280963,-448.160457813588));
#34510=CARTESIAN_POINT('Ctrl Pts',(-50.1775246783738,49.9196065704169,-448.134301683965));
#34511=CARTESIAN_POINT('Ctrl Pts',(-50.19858053573,49.9341074030923,-448.108144898866));
#34512=CARTESIAN_POINT('Ctrl Pts',(-50.2196315004226,49.9486139968755,-448.08198707884));
#34513=CARTESIAN_POINT('Ctrl Pts',(-50.2458115689115,49.9666551472137,-448.049455860921));
#34514=CARTESIAN_POINT('Ctrl Pts',(-50.2719831172911,49.9847063605971,-448.016922821836));
#34515=CARTESIAN_POINT('Ctrl Pts',(-50.2981526027619,50.0027598433546,-447.984389433468));
#34516=CARTESIAN_POINT('Ctrl Pts',(-51.2056740721611,50.6288295923436,-446.856176635811));
#34517=CARTESIAN_POINT('Ctrl Pts',(-52.1120994148901,51.2559476168219,-445.72786540226));
#34518=CARTESIAN_POINT('Ctrl Pts',(-53.0186423037857,51.8829276235022,-444.599574048826));
#34519=CARTESIAN_POINT('Ctrl Pts',(-53.0232182669799,51.8860924350838,-444.593878764279));
#34520=CARTESIAN_POINT('Ctrl Pts',(-53.0277942360827,51.8892572397411,-444.588183480956));
#34521=CARTESIAN_POINT('Ctrl Pts',(-53.0323702113011,51.8924220372635,-444.582488198884));
#34522=CARTESIAN_POINT('Ctrl Pts',(-53.0330339663677,51.8928810979642,-444.581662085947));
#34523=CARTESIAN_POINT('Ctrl Pts',(-53.0336977215629,51.8933401585148,-444.580835973034));
#34524=CARTESIAN_POINT('Ctrl Pts',(-53.0346051048533,51.8939677146664,-444.579706639678));
#34525=CARTESIAN_POINT('Ctrl Pts',(-53.034848732837,51.8941362103973,-444.579403419211));
#34526=CARTESIAN_POINT('Ctrl Pts',(-53.9910334341756,52.55544369592,-443.389331802383));
#34527=CARTESIAN_POINT('Ctrl Pts',(-54.9472421448168,53.2162725675843,-442.199619058995));
#34528=CARTESIAN_POINT('Ctrl Pts',(-55.9062274602824,53.8789834895428,-441.006551677525));
#34529=CARTESIAN_POINT('Ctrl Pts',(-55.9088457257679,53.8807928528758,-441.003294311226));
#34530=CARTESIAN_POINT('Ctrl Pts',(-55.9691684238764,53.9224790999222,-440.928247269069));
#34531=CARTESIAN_POINT('Ctrl Pts',(-56.0268728553218,53.962355983091,-440.856457593954));
#34532=CARTESIAN_POINT('Ctrl Pts',(-56.0845772867672,54.0022328662598,-440.784667918839));
#34533=CARTESIAN_POINT('Ctrl Pts',(-38.0485358858946,42.4342626183073,-462.49999999999));
#34534=CARTESIAN_POINT('Ctrl Pts',(-39.0356229365182,43.0696980016412,-461.308013965751));
#34535=CARTESIAN_POINT('Ctrl Pts',(-40.024611351385,43.7058204031952,-460.117292961907));
#34536=CARTESIAN_POINT('Ctrl Pts',(-41.0122388620067,44.3416392648618,-458.925224977469));
#34537=CARTESIAN_POINT('Ctrl Pts',(-41.0538006334439,44.3683960713702,-458.875059852891));
#34538=CARTESIAN_POINT('Ctrl Pts',(-41.0953600222231,44.3951523559108,-458.824892357397));
#34539=CARTESIAN_POINT('Ctrl Pts',(-41.1369165959835,44.4219078194676,-458.774722170664));
#34540=CARTESIAN_POINT('Ctrl Pts',(-41.6151691571787,44.729822255478,-458.197340107383));
#34541=CARTESIAN_POINT('Ctrl Pts',(-42.0930406432342,45.0376232051348,-457.619597236635));
#34542=CARTESIAN_POINT('Ctrl Pts',(-42.5698361712411,45.3448341513233,-457.040986313764));
#34543=CARTESIAN_POINT('Ctrl Pts',(-42.8053220530903,45.4965634279782,-456.755214540715));
#34544=CARTESIAN_POINT('Ctrl Pts',(-43.0367606506595,45.6544693989459,-456.469171724908));
#34545=CARTESIAN_POINT('Ctrl Pts',(-43.2678916148795,45.8122303117749,-456.182896741484));
#34546=CARTESIAN_POINT('Ctrl Pts',(-43.4934444669871,45.9661838244933,-455.903530715316));
#34547=CARTESIAN_POINT('Ctrl Pts',(-43.7177199550653,46.1216144233747,-455.623918373332));
#34548=CARTESIAN_POINT('Ctrl Pts',(-43.9405112854632,46.2787488604059,-455.344024006501));
#34549=CARTESIAN_POINT('Ctrl Pts',(-44.2274059719884,46.481095311562,-454.983596127692));
#34550=CARTESIAN_POINT('Ctrl Pts',(-44.5116147019647,46.6865336179401,-454.622656992109));
#34551=CARTESIAN_POINT('Ctrl Pts',(-44.7940809283859,46.8939195056093,-454.261399114584));
#34552=CARTESIAN_POINT('Ctrl Pts',(-45.4495870029688,47.3751901724509,-453.423044964395));
#34553=CARTESIAN_POINT('Ctrl Pts',(-46.0973324307058,47.8649979689372,-452.583283464107));
#34554=CARTESIAN_POINT('Ctrl Pts',(-46.750484847807,48.3475659606927,-451.744900168167));
#34555=CARTESIAN_POINT('Ctrl Pts',(-47.1434272238412,48.637883210256,-451.240521227343));
#34556=CARTESIAN_POINT('Ctrl Pts',(-47.5380826456442,48.9259784554183,-450.73658927729));
#34557=CARTESIAN_POINT('Ctrl Pts',(-47.9336785752366,49.2128162688131,-450.232930506939));
#34558=CARTESIAN_POINT('Ctrl Pts',(-48.4766346637746,49.60650165725,-449.541657985025));
#34559=CARTESIAN_POINT('Ctrl Pts',(-49.0208509935435,49.9984361157421,-448.850787354041));
#34560=CARTESIAN_POINT('Ctrl Pts',(-49.5650274806359,50.3902365781675,-448.160009139721));
#34561=CARTESIAN_POINT('Ctrl Pts',(-49.5655523325958,50.3906144652049,-448.159342892082));
#34562=CARTESIAN_POINT('Ctrl Pts',(-49.5660771826899,50.3909923543223,-448.158676644111));
#34563=CARTESIAN_POINT('Ctrl Pts',(-49.5666020308868,50.3913702455573,-448.158010395802));
#34564=CARTESIAN_POINT('Ctrl Pts',(-49.5871999259553,50.4062007509343,-448.13186319202));
#34565=CARTESIAN_POINT('Ctrl Pts',(-49.6077947898249,50.4210346498013,-448.105715441795));
#34566=CARTESIAN_POINT('Ctrl Pts',(-49.628385178826,50.4358736949496,-448.079566806258));
#34567=CARTESIAN_POINT('Ctrl Pts',(-49.6539924515631,50.4543282990007,-448.047047010645));
#34568=CARTESIAN_POINT('Ctrl Pts',(-49.6795919556881,50.4727918877815,-448.014525649639));
#34569=CARTESIAN_POINT('Ctrl Pts',(-49.7051894407867,50.4912575287471,-447.982004029836));
#34570=CARTESIAN_POINT('Ctrl Pts',(-50.5928747304147,51.1316203528912,-446.854199349668));
#34571=CARTESIAN_POINT('Ctrl Pts',(-51.4793636318734,51.7729560277259,-445.726369506217));
#34572=CARTESIAN_POINT('Ctrl Pts',(-52.3659887730324,52.4141980326467,-444.598510963065));
#34573=CARTESIAN_POINT('Ctrl Pts',(-52.3704641972652,52.4174348346216,-444.592817863218));
#34574=CARTESIAN_POINT('Ctrl Pts',(-52.3749396275605,52.4206716311789,-444.587124763277));
#34575=CARTESIAN_POINT('Ctrl Pts',(-52.379415064135,52.42390842213,-444.581431663254));
#34576=CARTESIAN_POINT('Ctrl Pts',(-52.3800642358547,52.4243779256327,-444.580605866827));
#34577=CARTESIAN_POINT('Ctrl Pts',(-52.3807134077064,52.4248474290174,-444.579780070399));
#34578=CARTESIAN_POINT('Ctrl Pts',(-52.3816008549171,52.4254892610355,-444.57865116965));
#34579=CARTESIAN_POINT('Ctrl Pts',(-52.3818391301617,52.4256615897709,-444.578348065331));
#34580=CARTESIAN_POINT('Ctrl Pts',(-53.3170155448827,53.1020127665171,-443.388732293172));
#34581=CARTESIAN_POINT('Ctrl Pts',(-54.2522286275839,53.777948100645,-442.199416824245));
#34582=CARTESIAN_POINT('Ctrl Pts',(-55.190351532113,54.4559698826095,-441.006592867525));
#34583=CARTESIAN_POINT('Ctrl Pts',(-55.1929128395437,54.4578210495521,-441.003336164678));
#34584=CARTESIAN_POINT('Ctrl Pts',(-55.2519233041263,54.5004704453264,-440.928304381204));
#34585=CARTESIAN_POINT('Ctrl Pts',(-55.3083724586708,54.5412686723922,-440.856529302479));
#34586=CARTESIAN_POINT('Ctrl Pts',(-55.3648216132152,54.5820668994579,-440.784754223754));
#34587=CARTESIAN_POINT('Ctrl Pts',(-37.7015139289768,42.6984598857191,-462.499999999992));
#34588=CARTESIAN_POINT('Ctrl Pts',(-38.6656677555457,43.3526547647935,-461.307627240141));
#34589=CARTESIAN_POINT('Ctrl Pts',(-39.6321479825285,44.0070708483155,-460.116339751994));
#34590=CARTESIAN_POINT('Ctrl Pts',(-40.5960403389216,44.6623261314753,-458.923599022175));
#34591=CARTESIAN_POINT('Ctrl Pts',(-40.6366032772516,44.6899008699457,-458.873405586832));
#34592=CARTESIAN_POINT('Ctrl Pts',(-40.6771616557822,44.7174771073708,-458.823209590049));
#34593=CARTESIAN_POINT('Ctrl Pts',(-40.7177150805053,44.7450546030494,-458.773010768619));
#34594=CARTESIAN_POINT('Ctrl Pts',(-41.184422931611,45.0624293706537,-458.195299163805));
#34595=CARTESIAN_POINT('Ctrl Pts',(-41.6504677956014,45.3799668296249,-457.617209805434));
#34596=CARTESIAN_POINT('Ctrl Pts',(-42.1152192455461,45.697282757234,-457.038325670186));
#34597=CARTESIAN_POINT('Ctrl Pts',(-42.3447566438694,45.8540028115309,-456.75241895951));
#34598=CARTESIAN_POINT('Ctrl Pts',(-42.5708216095122,46.015940864641,-456.466268917899));
#34599=CARTESIAN_POINT('Ctrl Pts',(-42.7965272793444,46.177825518152,-456.179908704162));
#34600=CARTESIAN_POINT('Ctrl Pts',(-43.0167857710584,46.335803249241,-455.900459504629));
#34601=CARTESIAN_POINT('Ctrl Pts',(-43.2358810096817,46.495077391614,-455.620789119718));
#34602=CARTESIAN_POINT('Ctrl Pts',(-43.4536348320486,46.6558385524204,-455.340868446679));
#34603=CARTESIAN_POINT('Ctrl Pts',(-43.7340425772515,46.8628552381805,-454.980406692624));
#34604=CARTESIAN_POINT('Ctrl Pts',(-44.0120383736682,47.072560028791,-454.619493541349));
#34605=CARTESIAN_POINT('Ctrl Pts',(-44.2884645672501,47.2839543133247,-454.25830384698));
#34606=CARTESIAN_POINT('Ctrl Pts',(-44.9299538219574,47.7745270780749,-453.420107926229));
#34607=CARTESIAN_POINT('Ctrl Pts',(-45.5643443466039,48.2725707246637,-452.580680637434));
#34608=CARTESIAN_POINT('Ctrl Pts',(-46.203310866777,48.7643743207005,-451.742523665027));
#34609=CARTESIAN_POINT('Ctrl Pts',(-46.5877188794695,49.0602477929697,-451.238280882478));
#34610=CARTESIAN_POINT('Ctrl Pts',(-46.9736034978234,49.3541840440922,-450.734458758233));
#34611=CARTESIAN_POINT('Ctrl Pts',(-47.3602852066659,49.6470247257858,-450.230896972499));
#34612=CARTESIAN_POINT('Ctrl Pts',(-47.8910065120105,50.0489490612078,-449.539757562139));
#34613=CARTESIAN_POINT('Ctrl Pts',(-48.4228027385423,50.4493248931892,-448.849014551141));
#34614=CARTESIAN_POINT('Ctrl Pts',(-48.954498800334,50.8495967064915,-448.158370168331));
#34615=CARTESIAN_POINT('Ctrl Pts',(-48.9550116150673,50.8499827640495,-448.157704049771));
#34616=CARTESIAN_POINT('Ctrl Pts',(-48.9555244281821,50.8503688233494,-448.157037930955));
#34617=CARTESIAN_POINT('Ctrl Pts',(-48.9560372396523,50.8507548844229,-448.156371811876));
#34618=CARTESIAN_POINT('Ctrl Pts',(-48.9761627481588,50.865906018653,-448.13022967979));
#34619=CARTESIAN_POINT('Ctrl Pts',(-48.9962856325201,50.8810599944751,-448.104087122759));
#34620=CARTESIAN_POINT('Ctrl Pts',(-49.0164046910113,50.8962182734208,-448.077943857189));
#34621=CARTESIAN_POINT('Ctrl Pts',(-49.0414257927484,50.9150698931336,-448.045430739947));
#34622=CARTESIAN_POINT('Ctrl Pts',(-49.066440270253,50.9339290234222,-448.012916363251));
#34623=CARTESIAN_POINT('Ctrl Pts',(-49.0914529239671,50.9527898809208,-447.980401815122));
#34624=CARTESIAN_POINT('Ctrl Pts',(-49.9588570721109,51.6068582664193,-446.852842370824));
#34625=CARTESIAN_POINT('Ctrl Pts',(-50.8250953085433,52.2617567039541,-445.725315370698));
#34626=CARTESIAN_POINT('Ctrl Pts',(-51.6914750408701,52.9165575812234,-444.597742047636));
#34627=CARTESIAN_POINT('Ctrl Pts',(-51.6958482722041,52.9198628244178,-444.592050387496));
#34628=CARTESIAN_POINT('Ctrl Pts',(-51.7002215093043,52.9231680625987,-444.586358726709));
#34629=CARTESIAN_POINT('Ctrl Pts',(-51.7045947523765,52.9264732956039,-444.580667065271));
#34630=CARTESIAN_POINT('Ctrl Pts',(-51.7052291007084,52.926952726774,-444.579841477514));
#34631=CARTESIAN_POINT('Ctrl Pts',(-51.7058634491659,52.9274321578352,-444.579015889744));
#34632=CARTESIAN_POINT('Ctrl Pts',(-51.7067306321233,52.9280875614446,-444.577887274224));
#34633=CARTESIAN_POINT('Ctrl Pts',(-51.7069634665143,52.928263534087,-444.577584246486));
#34634=CARTESIAN_POINT('Ctrl Pts',(-52.6207857604491,53.6189162247599,-443.388269030704));
#34635=CARTESIAN_POINT('Ctrl Pts',(-53.5346367726972,54.3091680481,-442.199229111192));
#34636=CARTESIAN_POINT('Ctrl Pts',(-54.4513541348557,55.0016680018326,-441.00663068191));
#34637=CARTESIAN_POINT('Ctrl Pts',(-54.453857000037,55.0035586986396,-441.00337459443));
#34638=CARTESIAN_POINT('Ctrl Pts',(-54.5115210061605,55.0471188509615,-440.928356979771));
#34639=CARTESIAN_POINT('Ctrl Pts',(-54.5666821443815,55.0887883037915,-440.856595454873));
#34640=CARTESIAN_POINT('Ctrl Pts',(-54.6218432826024,55.1304577566214,-440.784833929974));
#34641=CARTESIAN_POINT('Ctrl Pts',(-37.6313113290433,42.751907037111,-462.499999999992));
#34642=CARTESIAN_POINT('Ctrl Pts',(-38.5908257605495,43.4098969653116,-461.307549005485));
#34643=CARTESIAN_POINT('Ctrl Pts',(-39.5527525773585,44.068013863756,-460.116146917469));
#34644=CARTESIAN_POINT('Ctrl Pts',(-40.5118433080807,44.727201138235,-458.923270091147));
#34645=CARTESIAN_POINT('Ctrl Pts',(-40.5522041823061,44.7549413444782,-458.873070928532));
#34646=CARTESIAN_POINT('Ctrl Pts',(-40.5925600562959,44.782683458509,-458.822869165933));
#34647=CARTESIAN_POINT('Ctrl Pts',(-40.6329105438009,44.8104272514234,-458.772664551699));
#34648=CARTESIAN_POINT('Ctrl Pts',(-41.0972828981243,45.1297158456914,-458.194886280578));
#34649=CARTESIAN_POINT('Ctrl Pts',(-41.5609352344926,45.4492230021257,-457.616726827702));
#34650=CARTESIAN_POINT('Ctrl Pts',(-42.0232501654307,45.7685831691666,-457.037787421545));
#34651=CARTESIAN_POINT('Ctrl Pts',(-42.2515841845416,45.9263128586153,-456.751853412964));
#34652=CARTESIAN_POINT('Ctrl Pts',(-42.4765620635468,46.0890666026172,-456.465681679556));
#34653=CARTESIAN_POINT('Ctrl Pts',(-42.7011701954168,46.2517854895581,-456.179304223712));
#34654=CARTESIAN_POINT('Ctrl Pts',(-42.9203576371376,46.4105773206966,-455.899838198193));
#34655=CARTESIAN_POINT('Ctrl Pts',(-43.1384049104296,46.5706290125608,-455.620156071188));
#34656=CARTESIAN_POINT('Ctrl Pts',(-43.3551396440792,46.7321238601938,-455.340230076399));
#34657=CARTESIAN_POINT('Ctrl Pts',(-43.6342350799674,46.9400853351954,-454.979761469377));
#34658=CARTESIAN_POINT('Ctrl Pts',(-43.9109739988857,47.1506532362798,-454.618853574731));
#34659=CARTESIAN_POINT('Ctrl Pts',(-44.1861782928139,47.3628584201697,-454.257677673826));
#34660=CARTESIAN_POINT('Ctrl Pts',(-44.8248319425155,47.8553130008829,-453.419513762917));
#34661=CARTESIAN_POINT('Ctrl Pts',(-45.456520768033,48.3550227613251,-452.580154085162));
#34662=CARTESIAN_POINT('Ctrl Pts',(-46.0926174788846,48.8486947216528,-451.742042898044));
#34663=CARTESIAN_POINT('Ctrl Pts',(-46.4752989884454,49.145692218705,-451.237827660337));
#34664=CARTESIAN_POINT('Ctrl Pts',(-46.8594092717944,49.4408101063103,-450.734027753871));
#34665=CARTESIAN_POINT('Ctrl Pts',(-47.244287632288,49.7348651692648,-450.230485588141));
#34666=CARTESIAN_POINT('Ctrl Pts',(-47.7725338389458,50.1384562450403,-449.539373106272));
#34667=CARTESIAN_POINT('Ctrl Pts',(-48.3018174765153,50.5405397682904,-448.848655912817));
#34668=CARTESIAN_POINT('Ctrl Pts',(-48.830988746181,50.9425253372923,-448.158038604143));
#34669=CARTESIAN_POINT('Ctrl Pts',(-48.8314991257813,50.9429130477479,-448.157372511697));
#34670=CARTESIAN_POINT('Ctrl Pts',(-48.8320095038132,50.9433007598771,-448.156706419009));
#34671=CARTESIAN_POINT('Ctrl Pts',(-48.8325198802515,50.9436884737103,-448.156040326072));
#34672=CARTESIAN_POINT('Ctrl Pts',(-48.8525498248776,50.958904471211,-448.129899219992));
#34673=CARTESIAN_POINT('Ctrl Pts',(-48.8725772277053,50.9741231986547,-448.103757713546));
#34674=CARTESIAN_POINT('Ctrl Pts',(-48.8926009359556,50.989346058651,-448.077615534322));
#34675=CARTESIAN_POINT('Ctrl Pts',(-48.9175034552013,51.0082779946986,-448.045103768114));
#34676=CARTESIAN_POINT('Ctrl Pts',(-48.9423995817228,51.0272171431003,-448.012590804346));
#34677=CARTESIAN_POINT('Ctrl Pts',(-48.96729392395,51.0461579529697,-447.980077686819));
#34678=CARTESIAN_POINT('Ctrl Pts',(-49.8305951937789,51.7029989758228,-446.852567853776));
#34679=CARTESIAN_POINT('Ctrl Pts',(-50.6927367172891,52.3606411625206,-445.725102118905));
#34680=CARTESIAN_POINT('Ctrl Pts',(-51.5550208000225,53.0181850019341,-444.597586495915));
#34681=CARTESIAN_POINT('Ctrl Pts',(-51.559373357716,53.0215040907987,-444.591895127029));
#34682=CARTESIAN_POINT('Ctrl Pts',(-51.5637259211157,53.0248231747315,-444.586203757383));
#34683=CARTESIAN_POINT('Ctrl Pts',(-51.5680784904252,53.0281422535756,-444.580512386972));
#34684=CARTESIAN_POINT('Ctrl Pts',(-51.5687098399833,53.0286236931145,-444.579686841428));
#34685=CARTESIAN_POINT('Ctrl Pts',(-51.5693411896657,53.0291051325464,-444.57886129587));
#34686=CARTESIAN_POINT('Ctrl Pts',(-51.5702042731612,53.029763281691,-444.577732738052));
#34687=CARTESIAN_POINT('Ctrl Pts',(-51.5704360068666,53.0299399914963,-444.577429725806));
#34688=CARTESIAN_POINT('Ctrl Pts',(-52.4799383585943,53.7234858808289,-443.388175312629));
#34689=CARTESIAN_POINT('Ctrl Pts',(-53.3894678204164,54.4166339323314,-442.19919113681));
#34690=CARTESIAN_POINT('Ctrl Pts',(-54.3018548377726,55.1120628226348,-441.006638331766));
#34691=CARTESIAN_POINT('Ctrl Pts',(-54.3043458800771,55.1139615163399,-441.003382368775));
#34692=CARTESIAN_POINT('Ctrl Pts',(-54.361737497429,55.1577059148643,-440.928367620467));
#34693=CARTESIAN_POINT('Ctrl Pts',(-54.4166380697321,55.1995516168126,-440.856608837506));
#34694=CARTESIAN_POINT('Ctrl Pts',(-54.4715386420352,55.241397318761,-440.784850054546));
#34695=CARTESIAN_POINT('Ctrl Pts',(-37.5606381983877,42.8047320086185,-462.499999999992));
#34696=CARTESIAN_POINT('Ctrl Pts',(-38.5154836291893,43.4664771562781,-461.307471475064));
#34697=CARTESIAN_POINT('Ctrl Pts',(-39.4728284330313,44.1282446737561,-460.11595952772));
#34698=CARTESIAN_POINT('Ctrl Pts',(-40.4270726428532,44.7913302408702,-458.92295131962));
#34699=CARTESIAN_POINT('Ctrl Pts',(-40.4672295636733,44.8192344967634,-458.87274662814));
#34700=CARTESIAN_POINT('Ctrl Pts',(-40.5073810149251,44.847141098464,-458.822539298062));
#34701=CARTESIAN_POINT('Ctrl Pts',(-40.5475266184879,44.8750498302346,-458.77232908952));
#34702=CARTESIAN_POINT('Ctrl Pts',(-41.0095410722123,45.1962366182965,-458.194486436468));
#34703=CARTESIAN_POINT('Ctrl Pts',(-41.4707747128536,45.5177018945107,-457.616259201806));
#34704=CARTESIAN_POINT('Ctrl Pts',(-41.9306238174049,45.8391009011587,-457.037267245341));
#34705=CARTESIAN_POINT('Ctrl Pts',(-42.1577399825993,45.9978375588247,-456.751307282541));
#34706=CARTESIAN_POINT('Ctrl Pts',(-42.3816219841029,46.1613950630015,-456.465115401567));
#34707=CARTESIAN_POINT('Ctrl Pts',(-42.6051230311094,46.3249379193904,-456.178722323756));
#34708=CARTESIAN_POINT('Ctrl Pts',(-42.8232301063401,46.4845338343074,-455.89924105329));
#34709=CARTESIAN_POINT('Ctrl Pts',(-43.040221055301,46.6453518941958,-455.619548880493));
#34710=CARTESIAN_POINT('Ctrl Pts',(-43.2559295886666,46.8075678422351,-455.339619382112));
#34711=CARTESIAN_POINT('Ctrl Pts',(-43.533703557475,47.0164578985896,-454.979146263414));
#34712=CARTESIAN_POINT('Ctrl Pts',(-43.8091788928938,47.2278699183855,-454.618246243049));
#34713=CARTESIAN_POINT('Ctrl Pts',(-44.0831559855213,47.4408660030456,-454.257086717384));
#34714=CARTESIAN_POINT('Ctrl Pts',(-44.7189617269349,47.9351559899446,-453.418960807727));
#34715=CARTESIAN_POINT('Ctrl Pts',(-45.3479413476419,48.4364833568867,-452.579674012533));
#34716=CARTESIAN_POINT('Ctrl Pts',(-45.9811500955024,48.9319978078526,-451.741608611509));
#34717=CARTESIAN_POINT('Ctrl Pts',(-46.3620941805204,49.2301037638653,-451.237420919129));
#34718=CARTESIAN_POINT('Ctrl Pts',(-46.7444190537688,49.526390552976,-450.733642121788));
#34719=CARTESIAN_POINT('Ctrl Pts',(-47.1274832847747,49.8216487675473,-450.230117735052));
#34720=CARTESIAN_POINT('Ctrl Pts',(-47.6532395956147,50.2268911709703,-449.539029654883));
#34721=CARTESIAN_POINT('Ctrl Pts',(-48.1799972723325,50.6306687557846,-448.848334564663));
#34722=CARTESIAN_POINT('Ctrl Pts',(-48.7066317741023,51.0343542998095,-448.157740164373));
#34723=CARTESIAN_POINT('Ctrl Pts',(-48.7071397070192,51.0347436498714,-448.157074094021));
#34724=CARTESIAN_POINT('Ctrl Pts',(-48.7076476384221,51.0351330015347,-448.156408023443));
#34725=CARTESIAN_POINT('Ctrl Pts',(-48.708155568287,51.0355223548284,-448.155741952633));
#34726=CARTESIAN_POINT('Ctrl Pts',(-48.7280894960771,51.0508026936685,-448.129601714899));
#34727=CARTESIAN_POINT('Ctrl Pts',(-48.7480209714833,51.0660856444756,-448.103461101891));
#34728=CARTESIAN_POINT('Ctrl Pts',(-48.7679488930859,51.0813725479371,-448.077319852977));
#34729=CARTESIAN_POINT('Ctrl Pts',(-48.7927322871024,51.1003841317505,-448.04480924375));
#34730=CARTESIAN_POINT('Ctrl Pts',(-48.8175095360115,51.1194026135235,-448.012297500911));
#34731=CARTESIAN_POINT('Ctrl Pts',(-48.8422850463451,51.1384226866356,-447.979785621856));
#34732=CARTESIAN_POINT('Ctrl Pts',(-49.7014653908732,51.7980124488417,-446.852318737373));
#34733=CARTESIAN_POINT('Ctrl Pts',(-50.559497538848,52.4583717597448,-445.724906964639));
#34734=CARTESIAN_POINT('Ctrl Pts',(-51.4176727221505,53.1186299287702,-444.59744300476));
#34735=CARTESIAN_POINT('Ctrl Pts',(-51.4220045393222,53.1219627187762,-444.591751896654));
#34736=CARTESIAN_POINT('Ctrl Pts',(-51.4263363621208,53.1252955038863,-444.586060787705));
#34737=CARTESIAN_POINT('Ctrl Pts',(-51.4306681907468,53.128628283949,-444.580369677911));
#34738=CARTESIAN_POINT('Ctrl Pts',(-51.431296531824,53.1291117108792,-444.57954417017));
#34739=CARTESIAN_POINT('Ctrl Pts',(-51.4319248730238,53.1295951377032,-444.578718662414));
#34740=CARTESIAN_POINT('Ctrl Pts',(-51.4327838437864,53.1302560037031,-444.577590156269));
#34741=CARTESIAN_POINT('Ctrl Pts',(-51.433014473243,53.1304334429709,-444.577287157896));
#34742=CARTESIAN_POINT('Ctrl Pts',(-52.3381828974584,53.8268423076476,-443.388087195484));
#34743=CARTESIAN_POINT('Ctrl Pts',(-53.2433759381523,54.5228543703159,-442.199153784258));
#34744=CARTESIAN_POINT('Ctrl Pts',(-54.1514103835472,55.2211781197432,-441.006645871012));
#34745=CARTESIAN_POINT('Ctrl Pts',(-54.1538895422346,55.2230847172935,-441.003390030542));
#34746=CARTESIAN_POINT('Ctrl Pts',(-54.211007370146,55.2670112178498,-440.928378103979));
#34747=CARTESIAN_POINT('Ctrl Pts',(-54.2656460366574,55.3090311178125,-440.856622020288));
#34748=CARTESIAN_POINT('Ctrl Pts',(-54.3202847031689,55.351051017775,-440.784865936597));
#34749=CARTESIAN_POINT('Ctrl Pts',(-37.4895054223497,42.8569273733703,-462.499999999992));
#34750=CARTESIAN_POINT('Ctrl Pts',(-38.4396517070487,43.5223865535762,-461.30739452007));
#34751=CARTESIAN_POINT('Ctrl Pts',(-39.3923845302881,44.1877558922935,-460.115776989513));
#34752=CARTESIAN_POINT('Ctrl Pts',(-40.3417425663939,44.854700825913,-458.922642054846));
#34753=CARTESIAN_POINT('Ctrl Pts',(-40.3816938651216,44.8827674933499,-458.872432030404));
#34754=CARTESIAN_POINT('Ctrl Pts',(-40.4216392077703,44.9108369620788,-458.822219329407));
#34755=CARTESIAN_POINT('Ctrl Pts',(-40.4615782246053,44.9389090304533,-458.772003723843));
#34756=CARTESIAN_POINT('Ctrl Pts',(-40.9212151812771,45.2619755728383,-458.194098959325));
#34757=CARTESIAN_POINT('Ctrl Pts',(-41.3800082970933,45.5853829698017,-457.615806314063));
#34758=CARTESIAN_POINT('Ctrl Pts',(-41.8373679432734,45.9088086873809,-457.03676440528));
#34759=CARTESIAN_POINT('Ctrl Pts',(-42.063254582884,46.0685463229984,-456.750779771391));
#34760=CARTESIAN_POINT('Ctrl Pts',(-42.2860324560788,46.2328960939693,-456.464569141792));
#34761=CARTESIAN_POINT('Ctrl Pts',(-42.5084177401601,46.3972524853508,-456.178161869978));
#34762=CARTESIAN_POINT('Ctrl Pts',(-42.7254359802761,46.5576423014161,-455.898666748067));
#34763=CARTESIAN_POINT('Ctrl Pts',(-42.941362733517,46.7192159075507,-455.618965976344));
#34764=CARTESIAN_POINT('Ctrl Pts',(-43.1560379722264,46.8821413693933,-455.339034467228));
#34765=CARTESIAN_POINT('Ctrl Pts',(-43.4324813383313,47.091945086705,-454.97855875925));
#34766=CARTESIAN_POINT('Ctrl Pts',(-43.7066854724977,47.3041847647207,-454.617668656292));
#34767=CARTESIAN_POINT('Ctrl Pts',(-43.9794286502786,47.5179548513687,-454.256527458661));
#34768=CARTESIAN_POINT('Ctrl Pts',(-44.6123709035941,48.0140410282453,-453.418444082009));
#34769=CARTESIAN_POINT('Ctrl Pts',(-45.2386289538674,48.5169464151524,-452.579233899357));
#34770=CARTESIAN_POINT('Ctrl Pts',(-45.8689315080284,49.0142786796981,-451.741214186485));
#34771=CARTESIAN_POINT('Ctrl Pts',(-46.2481272007452,49.3134782487302,-451.237053980509));
#34772=CARTESIAN_POINT('Ctrl Pts',(-46.6286559997937,49.6109208470317,-450.733295367014));
#34773=CARTESIAN_POINT('Ctrl Pts',(-47.0098959158467,49.9073700575108,-450.229787248531));
#34774=CARTESIAN_POINT('Ctrl Pts',(-47.5331483513002,50.3142471048499,-449.538721496565));
#34775=CARTESIAN_POINT('Ctrl Pts',(-48.0573675108946,50.7197032017148,-448.848045448175));
#34776=CARTESIAN_POINT('Ctrl Pts',(-48.5814538539718,51.1250730868311,-448.157470490684));
#34777=CARTESIAN_POINT('Ctrl Pts',(-48.5819593292189,51.1254640614206,-448.156804439085));
#34778=CARTESIAN_POINT('Ctrl Pts',(-48.5824648030095,51.1258550375369,-448.156138387274));
#34779=CARTESIAN_POINT('Ctrl Pts',(-48.5829702753206,51.1262460152077,-448.155472335249));
#34780=CARTESIAN_POINT('Ctrl Pts',(-48.6028077553457,51.1415901034307,-448.129332834687));
#34781=CARTESIAN_POINT('Ctrl Pts',(-48.6226428771039,51.1569366818667,-448.103192984056));
#34782=CARTESIAN_POINT('Ctrl Pts',(-48.6424745919669,51.1722870274805,-448.077052534873));
#34783=CARTESIAN_POINT('Ctrl Pts',(-48.6671383383061,51.1913775112361,-448.044542920233));
#34784=CARTESIAN_POINT('Ctrl Pts',(-48.6917961975074,51.2104745688835,-448.012032236872));
#34785=CARTESIAN_POINT('Ctrl Pts',(-48.7164523682614,51.229573145118,-447.979521434495));
#34786=CARTESIAN_POINT('Ctrl Pts',(-49.5714941816486,51.8918852867524,-446.852091887728));
#34787=CARTESIAN_POINT('Ctrl Pts',(-50.4254033950816,52.5549337315204,-445.724727758715));
#34788=CARTESIAN_POINT('Ctrl Pts',(-51.2794555464531,53.2178767746817,-444.597310199858));
#34789=CARTESIAN_POINT('Ctrl Pts',(-51.2837665517663,53.2212231171466,-444.59161932597));
#34790=CARTESIAN_POINT('Ctrl Pts',(-51.2880775626097,53.2245694547171,-444.585928451187));
#34791=CARTESIAN_POINT('Ctrl Pts',(-51.2923885791803,53.2279157872473,-444.580237575499));
#34792=CARTESIAN_POINT('Ctrl Pts',(-51.293013901424,53.2284011799921,-444.579412101718));
#34793=CARTESIAN_POINT('Ctrl Pts',(-51.2936392237882,53.2288865726309,-444.578586627916));
#34794=CARTESIAN_POINT('Ctrl Pts',(-51.2944940676643,53.229550125988,-444.577458168189));
#34795=CARTESIAN_POINT('Ctrl Pts',(-51.2947235890718,53.229728286798,-444.577155182282));
#34796=CARTESIAN_POINT('Ctrl Pts',(-52.1955431706003,53.9289690413498,-443.388004133628));
#34797=CARTESIAN_POINT('Ctrl Pts',(-53.096384092799,54.6278125449327,-442.199117108152));
#34798=CARTESIAN_POINT('Ctrl Pts',(-54.0000443626148,55.3289968257504,-441.006653315026));
#34799=CARTESIAN_POINT('Ctrl Pts',(-54.0025115786581,55.3309112334103,-441.003397594997));
#34800=CARTESIAN_POINT('Ctrl Pts',(-54.0593542561864,55.3750176761223,-440.928388442925));
#34801=CARTESIAN_POINT('Ctrl Pts',(-54.1137297150346,55.4172097079706,-440.8566350133));
#34802=CARTESIAN_POINT('Ctrl Pts',(-54.1681051738827,55.459401739819,-440.784881583676));
#34803=CARTESIAN_POINT('Ctrl Pts',(-37.2083128059277,43.0632591376727,-462.499999999992));
#34804=CARTESIAN_POINT('Ctrl Pts',(-38.1398830521092,43.7434001366877,-461.307090311834));
#34805=CARTESIAN_POINT('Ctrl Pts',(-39.0743844078769,44.42300771542,-460.115055403785));
#34806=CARTESIAN_POINT('Ctrl Pts',(-40.0044270728122,45.1052089826993,-458.921419510532));
#34807=CARTESIAN_POINT('Ctrl Pts',(-40.0435655336703,45.13391767382,-458.871188404532));
#34808=CARTESIAN_POINT('Ctrl Pts',(-40.0826961152396,45.1626309667934,-458.820954471935));
#34809=CARTESIAN_POINT('Ctrl Pts',(-40.121818480937,45.1913487156767,-458.770717531581));
#34810=CARTESIAN_POINT('Ctrl Pts',(-40.5720570329071,45.5218460524969,-458.19256723629));
#34811=CARTESIAN_POINT('Ctrl Pts',(-41.0212025910257,45.8529307825446,-457.614016018555));
#34812=CARTESIAN_POINT('Ctrl Pts',(-41.4687212419307,46.1843682238502,-457.034776644924));
#34813=CARTESIAN_POINT('Ctrl Pts',(-41.6897474847581,46.3480627921904,-456.748694484566));
#34814=CARTESIAN_POINT('Ctrl Pts',(-41.9081606649748,46.5155444467336,-456.462409740401));
#34815=CARTESIAN_POINT('Ctrl Pts',(-42.1261352636642,46.6831167962974,-456.175946358746));
#34816=CARTESIAN_POINT('Ctrl Pts',(-42.3388492658203,46.846644956646,-455.896396481149));
#34817=CARTESIAN_POINT('Ctrl Pts',(-42.550569182276,47.0112052875742,-455.616661717296));
#34818=CARTESIAN_POINT('Ctrl Pts',(-42.7611597381693,47.1769355048875,-455.33672225961));
#34819=CARTESIAN_POINT('Ctrl Pts',(-43.0323431428835,47.3903509850093,-454.976236316035));
#34820=CARTESIAN_POINT('Ctrl Pts',(-43.3015221335637,47.6058624512679,-454.615385417249));
#34821=CARTESIAN_POINT('Ctrl Pts',(-43.5693875635118,47.8226922194896,-454.254316671561));
#34822=CARTESIAN_POINT('Ctrl Pts',(-44.1910102570514,48.3258788553598,-453.41640143072));
#34823=CARTESIAN_POINT('Ctrl Pts',(-44.8065097575579,48.8350222606245,-452.577494102567));
#34824=CARTESIAN_POINT('Ctrl Pts',(-45.425323933847,49.3395404637074,-451.739654998012));
#34825=CARTESIAN_POINT('Ctrl Pts',(-45.7976081149786,49.643063158076,-451.235603447626));
#34826=CARTESIAN_POINT('Ctrl Pts',(-46.1710369127103,49.9450747473344,-450.731924622224));
#34827=CARTESIAN_POINT('Ctrl Pts',(-46.5450651898624,50.2462320442134,-450.228480813228));
#34828=CARTESIAN_POINT('Ctrl Pts',(-47.058419638616,50.6595709481716,-449.537503326142));
#34829=CARTESIAN_POINT('Ctrl Pts',(-47.5726038704107,51.0716623153226,-448.846902551382));
#34830=CARTESIAN_POINT('Ctrl Pts',(-48.0866171719202,51.4836905133122,-448.156404452575));
#34831=CARTESIAN_POINT('Ctrl Pts',(-48.0871129318347,51.4840879097679,-448.155738475105));
#34832=CARTESIAN_POINT('Ctrl Pts',(-48.0876086905194,51.4844853074556,-448.155072497485));
#34833=CARTESIAN_POINT('Ctrl Pts',(-48.0881044479561,51.4848827063976,-448.154406519712));
#34834=CARTESIAN_POINT('Ctrl Pts',(-48.1075606635219,51.5004788001911,-448.128269933244));
#34835=CARTESIAN_POINT('Ctrl Pts',(-48.1270148928715,51.5160769028946,-448.10213309634));
#34836=CARTESIAN_POINT('Ctrl Pts',(-48.1464662960652,51.5316780395761,-448.075995808548));
#34837=CARTESIAN_POINT('Ctrl Pts',(-48.1706570671417,51.5510804200746,-448.043490125577));
#34838=CARTESIAN_POINT('Ctrl Pts',(-48.1948429708511,51.5704880934038,-448.010983630402));
#34839=CARTESIAN_POINT('Ctrl Pts',(-48.2190273842736,51.5898969977258,-447.978477084207));
#34840=CARTESIAN_POINT('Ctrl Pts',(-49.0577093075446,52.2629708871368,-446.85119513592));
#34841=CARTESIAN_POINT('Ctrl Pts',(-49.8953202852591,52.9366496577472,-445.724019345728));
#34842=CARTESIAN_POINT('Ctrl Pts',(-50.7330738159265,53.610206187758,-444.596785213209));
#34843=CARTESIAN_POINT('Ctrl Pts',(-50.7373025505724,53.6136061039984,-444.591095265205));
#34844=CARTESIAN_POINT('Ctrl Pts',(-50.7415312903665,53.6170060153503,-444.585405316087));
#34845=CARTESIAN_POINT('Ctrl Pts',(-50.7457600354915,53.6204059216904,-444.579715365841));
#34846=CARTESIAN_POINT('Ctrl Pts',(-50.7463734240847,53.6208990854317,-444.578890026296));
#34847=CARTESIAN_POINT('Ctrl Pts',(-50.7469868127902,53.6213922490676,-444.578064686727));
#34848=CARTESIAN_POINT('Ctrl Pts',(-50.7478253428082,53.6220664257269,-444.576936410497));
#34849=CARTESIAN_POINT('Ctrl Pts',(-50.7480504840236,53.6222474388418,-444.576633473854));
#34850=CARTESIAN_POINT('Ctrl Pts',(-51.6316787998422,54.3326828432827,-443.387675784562));
#34851=CARTESIAN_POINT('Ctrl Pts',(-52.5153155068425,55.0427192219841,-442.198972125054));
#34852=CARTESIAN_POINT('Ctrl Pts',(-53.401684368333,55.7552113745149,-441.006682741713));
#34853=CARTESIAN_POINT('Ctrl Pts',(-53.4041043743063,55.7571566560599,-441.003427497796));
#34854=CARTESIAN_POINT('Ctrl Pts',(-53.4598593639825,55.8019744221367,-440.928429313338));
#34855=CARTESIAN_POINT('Ctrl Pts',(-53.5131943453476,55.8448469028314,-440.856686375285));
#34856=CARTESIAN_POINT('Ctrl Pts',(-53.5665293267126,55.8877193835262,-440.784943437231));
#34857=CARTESIAN_POINT('Ctrl Pts',(-36.9199317767795,43.2597666774808,-462.499999999992));
#34858=CARTESIAN_POINT('Ctrl Pts',(-37.8324549102319,43.9539458782433,-461.306795095633));
#34859=CARTESIAN_POINT('Ctrl Pts',(-38.7482571578729,44.647027599901,-460.114409634641));
#34860=CARTESIAN_POINT('Ctrl Pts',(-39.658365681366,45.3438748510546,-458.920345532314));
#34861=CARTESIAN_POINT('Ctrl Pts',(-39.6966652649939,45.3731998808534,-458.870096406233));
#34862=CARTESIAN_POINT('Ctrl Pts',(-39.7349547780735,45.4025315850734,-458.81984431378));
#34863=CARTESIAN_POINT('Ctrl Pts',(-39.7732339211675,45.4318698879971,-458.769589121741));
#34864=CARTESIAN_POINT('Ctrl Pts',(-40.2137682715346,45.7695088520574,-458.191228777496));
#34865=CARTESIAN_POINT('Ctrl Pts',(-40.6529256329602,46.108019773596,-457.612456043251));
#34866=CARTESIAN_POINT('Ctrl Pts',(-41.0902344735065,46.44727828479,-457.033059804923));
#34867=CARTESIAN_POINT('Ctrl Pts',(-41.3062181644335,46.6148356232938,-456.74690017022));
#34868=CARTESIAN_POINT('Ctrl Pts',(-41.5201379527339,46.7852690047599,-456.460563173376));
#34869=CARTESIAN_POINT('Ctrl Pts',(-41.7335664838255,46.9558937191734,-456.174065997285));
#34870=CARTESIAN_POINT('Ctrl Pts',(-41.9418441331284,47.1224005786326,-455.894483140846));
#34871=CARTESIAN_POINT('Ctrl Pts',(-42.1492344243933,47.2897780164087,-455.614736995588));
#34872=CARTESIAN_POINT('Ctrl Pts',(-42.355629639368,47.4581314476689,-455.334812918698));
#34873=CARTESIAN_POINT('Ctrl Pts',(-42.6214105851287,47.6749249144548,-454.974346781408));
#34874=CARTESIAN_POINT('Ctrl Pts',(-42.8854456343389,47.8934503728073,-454.613567015252));
#34875=CARTESIAN_POINT('Ctrl Pts',(-43.1483286166096,48.1130752521023,-454.252601238184));
#34876=CARTESIAN_POINT('Ctrl Pts',(-43.7583887783723,48.6227483706607,-453.414924951775));
#34877=CARTESIAN_POINT('Ctrl Pts',(-44.3629368138195,49.1375104332791,-452.576378766951));
#34878=CARTESIAN_POINT('Ctrl Pts',(-44.9699777257463,49.6488289529857,-451.738718740192));
#34879=CARTESIAN_POINT('Ctrl Pts',(-45.3351790050144,49.9564427790748,-451.234774924621));
#34880=CARTESIAN_POINT('Ctrl Pts',(-45.70134058345,50.2628191175988,-450.731161428449));
#34881=CARTESIAN_POINT('Ctrl Pts',(-46.067997071373,50.5684951457719,-450.227758321355));
#34882=CARTESIAN_POINT('Ctrl Pts',(-46.5712337268281,50.9880360161434,-449.5368366977));
#34883=CARTESIAN_POINT('Ctrl Pts',(-47.0751846899181,51.4065209593756,-448.846263357661));
#34884=CARTESIAN_POINT('Ctrl Pts',(-47.5789444621768,51.8249646754256,-448.155787962735));
#34885=CARTESIAN_POINT('Ctrl Pts',(-47.5794303326803,51.8253682595746,-448.155122007162));
#34886=CARTESIAN_POINT('Ctrl Pts',(-47.5799162022267,51.8257718446248,-448.154456051502));
#34887=CARTESIAN_POINT('Ctrl Pts',(-47.5804020708026,51.8261754305922,-448.153790095752));
#34888=CARTESIAN_POINT('Ctrl Pts',(-47.5994701937419,51.8420143368808,-448.127654373588));
#34889=CARTESIAN_POINT('Ctrl Pts',(-47.6185367754878,51.8578547120417,-448.101518502401));
#34890=CARTESIAN_POINT('Ctrl Pts',(-47.6376012071881,51.8736973011133,-448.075382335517));
#34891=CARTESIAN_POINT('Ctrl Pts',(-47.6613107205006,51.8933999642927,-448.042878046564));
#34892=CARTESIAN_POINT('Ctrl Pts',(-47.6850165472328,51.9131064885463,-448.01037321669));
#34893=CARTESIAN_POINT('Ctrl Pts',(-47.70872115003,51.9328139156338,-447.977868398389));
#34894=CARTESIAN_POINT('Ctrl Pts',(-48.5307639061233,52.6162401606172,-446.850646371043));
#34895=CARTESIAN_POINT('Ctrl Pts',(-49.351859747534,53.3001149112981,-445.723560185446));
#34896=CARTESIAN_POINT('Ctrl Pts',(-50.1730897445005,53.9838271096126,-444.596427251579));
#34897=CARTESIAN_POINT('Ctrl Pts',(-50.177235073184,53.9872782886944,-444.590737814395));
#34898=CARTESIAN_POINT('Ctrl Pts',(-50.1813804063884,53.9907294623442,-444.585048376292));
#34899=CARTESIAN_POINT('Ctrl Pts',(-50.185525744272,53.9941806304614,-444.579358937251));
#34900=CARTESIAN_POINT('Ctrl Pts',(-50.1861270344651,53.994681229834,-444.578533671858));
#34901=CARTESIAN_POINT('Ctrl Pts',(-50.1867283247567,53.9951818290902,-444.577708406444));
#34902=CARTESIAN_POINT('Ctrl Pts',(-50.1875503156819,53.9958661705609,-444.576580231593));
#34903=CARTESIAN_POINT('Ctrl Pts',(-50.18777101623,53.9960499128762,-444.576277322171));
#34904=CARTESIAN_POINT('Ctrl Pts',(-51.0539707121218,54.7171968052672,-443.387426468621));
#34905=CARTESIAN_POINT('Ctrl Pts',(-51.9201546955739,55.4379190446405,-442.198837749311));
#34906=CARTESIAN_POINT('Ctrl Pts',(-52.7888945371382,56.1611826490833,-441.006710716959));
#34907=CARTESIAN_POINT('Ctrl Pts',(-52.7912664106188,56.163157339747,-441.003455916653));
#34908=CARTESIAN_POINT('Ctrl Pts',(-52.8459124453165,56.2086526773579,-440.928467960805));
#34909=CARTESIAN_POINT('Ctrl Pts',(-52.8981866051577,56.2521733200442,-440.856734807396));
#34910=CARTESIAN_POINT('Ctrl Pts',(-52.9504607649989,56.2956939627305,-440.785001653987));
#34911=CARTESIAN_POINT('Ctrl Pts',(-36.6250350054762,43.44599737661,-462.499999999992));
#34912=CARTESIAN_POINT('Ctrl Pts',(-37.5180066093736,44.15348732022,-461.306500914477));
#34913=CARTESIAN_POINT('Ctrl Pts',(-38.4145575367227,44.8593642524127,-460.113803019785));
#34914=CARTESIAN_POINT('Ctrl Pts',(-39.3044366439474,45.5699226199423,-458.919379760096));
#34915=CARTESIAN_POINT('Ctrl Pts',(-39.3418849244615,45.5998246469174,-458.869115519798));
#34916=CARTESIAN_POINT('Ctrl Pts',(-39.3793213988626,45.6297349680817,-458.818848228504));
#34917=CARTESIAN_POINT('Ctrl Pts',(-39.4167458019573,45.659653565018,-458.768577792298));
#34918=CARTESIAN_POINT('Ctrl Pts',(-39.847443403123,46.0039708250165,-458.190042011011));
#34919=CARTESIAN_POINT('Ctrl Pts',(-40.2765397746495,46.3493827979472,-457.611088416315));
#34920=CARTESIAN_POINT('Ctrl Pts',(-40.7036203901279,46.6958551892692,-457.03156832762));
#34921=CARTESIAN_POINT('Ctrl Pts',(-40.9145524342622,46.8669754112811,-456.74534752411));
#34922=CARTESIAN_POINT('Ctrl Pts',(-41.1238833998925,47.0402069499242,-456.458971155554));
#34923=CARTESIAN_POINT('Ctrl Pts',(-41.3326840621497,47.2137094884313,-456.17245062354));
#34924=CARTESIAN_POINT('Ctrl Pts',(-41.536445531553,47.3830247186094,-455.892844974849));
#34925=CARTESIAN_POINT('Ctrl Pts',(-41.7394134450216,47.5530714696157,-455.613094645132));
#34926=CARTESIAN_POINT('Ctrl Pts',(-41.9415036422248,47.723927962429,-455.33318917845));
#34927=CARTESIAN_POINT('Ctrl Pts',(-42.2017408950516,47.9439446922492,-454.972747006051));
#34928=CARTESIAN_POINT('Ctrl Pts',(-42.4604567863254,48.1653822678638,-454.612034804759));
#34929=CARTESIAN_POINT('Ctrl Pts',(-42.7181653193154,48.3877287873109,-454.251163653175));
#34930=CARTESIAN_POINT('Ctrl Pts',(-43.3162173802191,48.9037178880493,-453.413706959669));
#34931=CARTESIAN_POINT('Ctrl Pts',(-43.9093206928263,49.4240297334006,-452.575484973039));
#34932=CARTESIAN_POINT('Ctrl Pts',(-44.5042986949365,49.9418368656499,-451.737996393529));
#34933=CARTESIAN_POINT('Ctrl Pts',(-44.8622428190275,50.2533542994772,-451.234155722167));
#34934=CARTESIAN_POINT('Ctrl Pts',(-45.2209889388158,50.5638744191451,-450.730604440263));
#34935=CARTESIAN_POINT('Ctrl Pts',(-45.5801392660453,50.8738318088303,-450.22723885709));
#34936=CARTESIAN_POINT('Ctrl Pts',(-46.0730737031377,51.2992488551844,-449.536368735082));
#34937=CARTESIAN_POINT('Ctrl Pts',(-46.5666196378205,51.723786943774,-448.845815383258));
#34938=CARTESIAN_POINT('Ctrl Pts',(-47.0599537059709,52.1483121119869,-448.155351859473));
#34939=CARTESIAN_POINT('Ctrl Pts',(-47.0604295210027,52.1487215616265,-448.154685915349));
#34940=CARTESIAN_POINT('Ctrl Pts',(-47.0609053353016,52.1491310119003,-448.154019971187));
#34941=CARTESIAN_POINT('Ctrl Pts',(-47.0613811488582,52.1495404628192,-448.153354026984));
#34942=CARTESIAN_POINT('Ctrl Pts',(-47.0800546582078,52.1656095416749,-448.12721875797));
#34943=CARTESIAN_POINT('Ctrl Pts',(-47.0987269925228,52.181679652834,-448.101083418635));
#34944=CARTESIAN_POINT('Ctrl Pts',(-47.1173977360254,52.1977513071622,-448.074947907397));
#34945=CARTESIAN_POINT('Ctrl Pts',(-47.1406176383329,52.2177388477424,-448.042444433842));
#34946=CARTESIAN_POINT('Ctrl Pts',(-47.1638348317754,52.2377290755748,-448.009940636929));
#34947=CARTESIAN_POINT('Ctrl Pts',(-47.1870510158254,52.257719953065,-447.9774368953));
#34948=CARTESIAN_POINT('Ctrl Pts',(-47.9921560870102,52.950975864979,-446.850252205454));
#34949=CARTESIAN_POINT('Ctrl Pts',(-48.7964083779301,53.6445747397623,-445.723217860489));
#34950=CARTESIAN_POINT('Ctrl Pts',(-49.6007898856695,54.3379719240151,-444.596151878923));
#34951=CARTESIAN_POINT('Ctrl Pts',(-49.6048501681102,54.3414719900715,-444.590462779695));
#34952=CARTESIAN_POINT('Ctrl Pts',(-49.6089104546008,54.3449720501023,-444.584773679848));
#34953=CARTESIAN_POINT('Ctrl Pts',(-49.6129707452809,54.3484721040223,-444.579084579361));
#34954=CARTESIAN_POINT('Ctrl Pts',(-49.6135596991939,54.348979794386,-444.578259363076));
#34955=CARTESIAN_POINT('Ctrl Pts',(-49.6141486531951,54.3494874846209,-444.577434146777));
#34956=CARTESIAN_POINT('Ctrl Pts',(-49.614953779844,54.3501815197612,-444.576306039075));
#34957=CARTESIAN_POINT('Ctrl Pts',(-49.6151699524152,54.3503678647776,-444.576003147684));
#34958=CARTESIAN_POINT('Ctrl Pts',(-50.4635983594652,55.0817297627234,-443.38722306242));
#34959=CARTESIAN_POINT('Ctrl Pts',(-51.3119941322142,55.8126389863823,-442.198718028092));
#34960=CARTESIAN_POINT('Ctrl Pts',(-52.1628056643231,56.5461223255794,-441.006738864584));
#34961=CARTESIAN_POINT('Ctrl Pts',(-52.1651285884545,56.5481249186544,-441.003484468476));
#34962=CARTESIAN_POINT('Ctrl Pts',(-52.2186468548831,56.594263105605,-440.92850583605));
#34963=CARTESIAN_POINT('Ctrl Pts',(-52.2698421964883,56.6383986951822,-440.856781601387));
#34964=CARTESIAN_POINT('Ctrl Pts',(-52.3210375380934,56.6825342847595,-440.785057366722));
#34965=CARTESIAN_POINT('Ctrl Pts',(-36.4766084300011,43.5397304642866,-462.499999999992));
#34966=CARTESIAN_POINT('Ctrl Pts',(-37.3597394155548,44.2539199318322,-461.306352848082));
#34967=CARTESIAN_POINT('Ctrl Pts',(-38.2466008250035,44.9662369117535,-460.11349770018));
#34968=CARTESIAN_POINT('Ctrl Pts',(-39.126298121938,45.6836963180454,-458.918893670464));
#34969=CARTESIAN_POINT('Ctrl Pts',(-39.163317927073,45.713888757542,-458.868621822924));
#34970=CARTESIAN_POINT('Ctrl Pts',(-39.2003250525556,45.7440903064847,-458.818346881794));
#34971=CARTESIAN_POINT('Ctrl Pts',(-39.2373192504284,45.7743009752964,-458.768068772937));
#34972=CARTESIAN_POINT('Ctrl Pts',(-39.6630658479214,46.1219795355618,-458.189444691194));
#34973=CARTESIAN_POINT('Ctrl Pts',(-40.0870983516069,46.4708649253793,-457.610400066349));
#34974=CARTESIAN_POINT('Ctrl Pts',(-40.5090309269309,46.8209681856273,-457.030817641651));
#34975=CARTESIAN_POINT('Ctrl Pts',(-40.7174203910613,46.9938816676861,-456.744566050838));
#34976=CARTESIAN_POINT('Ctrl Pts',(-40.9244417239637,47.1685215665686,-456.458169865827));
#34977=CARTESIAN_POINT('Ctrl Pts',(-41.1309131008923,47.3434725630331,-456.171637578378));
#34978=CARTESIAN_POINT('Ctrl Pts',(-41.3324014999132,47.5142012941004,-455.892020457959));
#34979=CARTESIAN_POINT('Ctrl Pts',(-41.5331435551981,47.6855915559898,-455.612268022131));
#34980=CARTESIAN_POINT('Ctrl Pts',(-41.7330669635199,47.8577078823811,-455.332371922285));
#34981=CARTESIAN_POINT('Ctrl Pts',(-41.9905139811264,48.0793469354703,-454.971941811825));
#34982=CARTESIAN_POINT('Ctrl Pts',(-42.2465526494743,48.3022502293791,-454.611263617082));
#34983=CARTESIAN_POINT('Ctrl Pts',(-42.5016567938734,48.5259665967417,-454.250440092116));
#34984=CARTESIAN_POINT('Ctrl Pts',(-43.0936649727752,49.045134639052,-453.413093923464));
#34985=CARTESIAN_POINT('Ctrl Pts',(-43.6810079611479,49.5682397847237,-452.575035111317));
#34986=CARTESIAN_POINT('Ctrl Pts',(-44.269914494973,50.0893127463512,-451.737632824132));
#34987=CARTESIAN_POINT('Ctrl Pts',(-44.6242059690676,50.4027949325426,-451.233844067009));
#34988=CARTESIAN_POINT('Ctrl Pts',(-44.9792197620226,50.7154006879465,-450.730324098608));
#34989=CARTESIAN_POINT('Ctrl Pts',(-45.3345921105317,51.0275129599142,-450.226977401865));
#34990=CARTESIAN_POINT('Ctrl Pts',(-45.8223412653823,51.4558875858787,-449.536133201512));
#34991=CARTESIAN_POINT('Ctrl Pts',(-46.3106501717744,51.8834723257838,-448.8455899101));
#34992=CARTESIAN_POINT('Ctrl Pts',(-46.7987368052008,52.3110583926103,-448.155132361262));
#34993=CARTESIAN_POINT('Ctrl Pts',(-46.7992075591422,52.3114707944515,-448.1544664229));
#34994=CARTESIAN_POINT('Ctrl Pts',(-46.7996783124634,52.3118831967924,-448.153800484525));
#34995=CARTESIAN_POINT('Ctrl Pts',(-46.8001490651575,52.3122955996415,-448.153134546134));
#34996=CARTESIAN_POINT('Ctrl Pts',(-46.8186239587558,52.3284805282765,-448.126999505198));
#34997=CARTESIAN_POINT('Ctrl Pts',(-46.8370978616136,52.3446662694824,-448.100864433553));
#34998=CARTESIAN_POINT('Ctrl Pts',(-46.8555704551306,52.3608532162617,-448.074729252314));
#34999=CARTESIAN_POINT('Ctrl Pts',(-46.8785439278674,52.3809841404973,-448.042226189162));
#35000=CARTESIAN_POINT('Ctrl Pts',(-46.9015151838398,52.4011171611805,-448.009722912155));
#35001=CARTESIAN_POINT('Ctrl Pts',(-46.9244855384026,52.4212507040935,-447.977219712434));
#35002=CARTESIAN_POINT('Ctrl Pts',(-47.7210655838424,53.1194540550525,-446.85005381519));
#35003=CARTESIAN_POINT('Ctrl Pts',(-48.5168402284758,53.817947247375,-445.723045562498));
#35004=CARTESIAN_POINT('Ctrl Pts',(-49.3127416041782,54.5162190502612,-444.596013279167));
#35005=CARTESIAN_POINT('Ctrl Pts',(-49.3167590813941,54.5197437219659,-444.590324350038));
#35006=CARTESIAN_POINT('Ctrl Pts',(-49.320776562423,54.5232683873462,-444.584635420441));
#35007=CARTESIAN_POINT('Ctrl Pts',(-49.3247940473947,54.5267930463247,-444.578946490355));
#35008=CARTESIAN_POINT('Ctrl Pts',(-49.3253767922476,54.5273043057051,-444.578121298786));
#35009=CARTESIAN_POINT('Ctrl Pts',(-49.3259595371832,54.5278155649508,-444.577296107207));
#35010=CARTESIAN_POINT('Ctrl Pts',(-49.3267561757542,54.5285144790801,-444.576168033304));
#35011=CARTESIAN_POINT('Ctrl Pts',(-49.3269700693174,54.5287021340803,-444.575865150988));
#35012=CARTESIAN_POINT('Ctrl Pts',(-50.166453883543,55.2652054185741,-443.387120684609));
#35013=CARTESIAN_POINT('Ctrl Pts',(-51.005896546406,56.0012419251978,-442.19865777036));
#35014=CARTESIAN_POINT('Ctrl Pts',(-51.847684454537,56.7398690312296,-441.006753031764));
#35015=CARTESIAN_POINT('Ctrl Pts',(-51.8499827416259,56.7418856680639,-441.003498839095));
#35016=CARTESIAN_POINT('Ctrl Pts',(-51.9029333830493,56.7883474120568,-440.928524899335));
#35017=CARTESIAN_POINT('Ctrl Pts',(-51.9535857370357,56.8327925148976,-440.856805153656));
#35018=CARTESIAN_POINT('Ctrl Pts',(-52.0042380910221,56.8772376177383,-440.785085407977));
#35019=CARTESIAN_POINT('Ctrl Pts',(-36.3265298420472,43.6308599885747,-462.499999999992));
#35020=CARTESIAN_POINT('Ctrl Pts',(-37.1996924263205,44.3515646943029,-461.306205043894));
#35021=CARTESIAN_POINT('Ctrl Pts',(-38.0767245769759,45.0701497336524,-460.113202298343));
#35022=CARTESIAN_POINT('Ctrl Pts',(-38.9461654620509,45.7942733563001,-458.918434989852));
#35023=CARTESIAN_POINT('Ctrl Pts',(-38.9827536523909,45.8247462422545,-458.868156271143));
#35024=CARTESIAN_POINT('Ctrl Pts',(-39.0193284050684,45.8552289382071,-458.817874430222));
#35025=CARTESIAN_POINT('Ctrl Pts',(-39.055889488618,45.8857214801469,-458.767589410541));
#35026=CARTESIAN_POINT('Ctrl Pts',(-39.4766516031382,46.2366439687069,-458.188885795776));
#35027=CARTESIAN_POINT('Ctrl Pts',(-39.8956019078602,46.588869745845,-457.60976043929));
#35028=CARTESIAN_POINT('Ctrl Pts',(-40.3123818868539,46.9424500599523,-457.030124041237));
#35029=CARTESIAN_POINT('Ctrl Pts',(-40.5182265207175,47.117080833903,-456.743845793373));
#35030=CARTESIAN_POINT('Ctrl Pts',(-40.7229140991737,47.2930901910441,-456.45743305462));
#35031=CARTESIAN_POINT('Ctrl Pts',(-40.9270355202662,47.4694454308959,-456.170891655718));
#35032=CARTESIAN_POINT('Ctrl Pts',(-41.1262306772588,47.6415445153561,-455.891265643742));
#35033=CARTESIAN_POINT('Ctrl Pts',(-41.3247234268514,47.814240849281,-455.611512924627));
#35034=CARTESIAN_POINT('Ctrl Pts',(-41.5224523086685,47.9875865726217,-455.331627009372));
#35035=CARTESIAN_POINT('Ctrl Pts',(-41.7770733725339,48.210808754874,-454.971210013896));
#35036=CARTESIAN_POINT('Ctrl Pts',(-42.0303904861937,48.4351519609238,-454.610564921474));
#35037=CARTESIAN_POINT('Ctrl Pts',(-42.2828416508517,48.6602195653475,-454.249786909219));
#35038=CARTESIAN_POINT('Ctrl Pts',(-42.8686931845577,49.1825233598961,-453.412546359771));
#35039=CARTESIAN_POINT('Ctrl Pts',(-43.4501509656181,49.7084043601187,-452.574641362324));
#35040=CARTESIAN_POINT('Ctrl Pts',(-44.0329126558366,50.2326641877339,-451.737323434432));
#35041=CARTESIAN_POINT('Ctrl Pts',(-44.3835073366807,50.5480636212026,-451.23358542862));
#35042=CARTESIAN_POINT('Ctrl Pts',(-44.7347523585696,50.8626983517476,-450.730095988748));
#35043=CARTESIAN_POINT('Ctrl Pts',(-45.0863145944221,51.1769041993063,-450.226767380469));
#35044=CARTESIAN_POINT('Ctrl Pts',(-45.5688343631488,51.6081522613428,-449.535948006564));
#35045=CARTESIAN_POINT('Ctrl Pts',(-46.051866847541,52.0386948751203,-448.8454129045));
#35046=CARTESIAN_POINT('Ctrl Pts',(-46.5346672429426,52.4692542469965,-448.154958604317));
#35047=CARTESIAN_POINT('Ctrl Pts',(-46.5351328983683,52.4696695165561,-448.154292669089));
#35048=CARTESIAN_POINT('Ctrl Pts',(-46.5355985532749,52.4700847864969,-448.153626733868));
#35049=CARTESIAN_POINT('Ctrl Pts',(-46.5360642076574,52.4705000568251,-448.15296079865));
#35050=CARTESIAN_POINT('Ctrl Pts',(-46.5543390158089,52.486797520918,-448.126825882315));
#35051=CARTESIAN_POINT('Ctrl Pts',(-46.5726129985307,52.5030956034475,-448.100690969133));
#35052=CARTESIAN_POINT('Ctrl Pts',(-46.590885924727,52.5193945911968,-448.074556000714));
#35053=CARTESIAN_POINT('Ctrl Pts',(-46.6136110808565,52.5396648553776,-448.04205320224));
#35054=CARTESIAN_POINT('Ctrl Pts',(-46.6363344623507,52.5599366896367,-448.009550285811));
#35055=CARTESIAN_POINT('Ctrl Pts',(-46.6590570386816,52.5802089368378,-447.97704746389));
#35056=CARTESIAN_POINT('Ctrl Pts',(-47.4470444786043,53.2832223601798,-446.849894668207));
#35057=CARTESIAN_POINT('Ctrl Pts',(-48.2342679927543,53.9864843524237,-445.722902977322));
#35058=CARTESIAN_POINT('Ctrl Pts',(-49.0216147906279,54.6895066857866,-444.595895746019));
#35059=CARTESIAN_POINT('Ctrl Pts',(-49.0255890868387,54.6930553367788,-444.590206943346));
#35060=CARTESIAN_POINT('Ctrl Pts',(-49.0295633866179,54.6966039811641,-444.584518140382));
#35061=CARTESIAN_POINT('Ctrl Pts',(-49.0335376900874,54.700152618871,-444.578829337106));
#35062=CARTESIAN_POINT('Ctrl Pts',(-49.0341141713702,54.7006673564177,-444.578004163932));
#35063=CARTESIAN_POINT('Ctrl Pts',(-49.0346906527306,54.7011820938238,-444.577178990751));
#35064=CARTESIAN_POINT('Ctrl Pts',(-49.035478728706,54.7018857627464,-444.576050942003));
#35065=CARTESIAN_POINT('Ctrl Pts',(-49.0356903232536,54.7020746943845,-444.575748066442));
#35066=CARTESIAN_POINT('Ctrl Pts',(-49.8661510191605,55.4435884902993,-443.387030112924));
#35067=CARTESIAN_POINT('Ctrl Pts',(-50.6965617967901,56.1846220730185,-442.19860142409));
#35068=CARTESIAN_POINT('Ctrl Pts',(-51.5292502964639,56.928253159528,-441.006767441799));
#35069=CARTESIAN_POINT('Ctrl Pts',(-51.5315237396241,56.9302834584019,-441.003513442585));
#35070=CARTESIAN_POINT('Ctrl Pts',(-51.5839019901038,56.9770599633293,-440.928543966134));
#35071=CARTESIAN_POINT('Ctrl Pts',(-51.6340067973954,57.0218061651152,-440.856828490035));
#35072=CARTESIAN_POINT('Ctrl Pts',(-51.6841116046869,57.0665523669012,-440.785113013937));
#35073=CARTESIAN_POINT('Ctrl Pts',(-36.1748926818072,43.719331120904,-462.499999999992));
#35074=CARTESIAN_POINT('Ctrl Pts',(-37.0379548305357,44.4463560888641,-461.30605648736));
#35075=CARTESIAN_POINT('Ctrl Pts',(-37.9050017202358,45.1710409795027,-460.112919510267));
#35076=CARTESIAN_POINT('Ctrl Pts',(-38.7641455383955,45.9015411849164,-458.918015765539));
#35077=CARTESIAN_POINT('Ctrl Pts',(-38.8003004030767,45.9322824130066,-458.86773130526));
#35078=CARTESIAN_POINT('Ctrl Pts',(-38.836441276667,45.9630339403556,-458.817443718184));
#35079=CARTESIAN_POINT('Ctrl Pts',(-38.8725679428437,45.9937958220965,-458.767152961549));
#35080=CARTESIAN_POINT('Ctrl Pts',(-39.288330578282,46.3478179995397,-458.188383323229));
#35081=CARTESIAN_POINT('Ctrl Pts',(-39.7022105061783,46.703211031918,-457.609193372195));
#35082=CARTESIAN_POINT('Ctrl Pts',(-40.1138740358445,47.0600563389859,-457.029515743679));
#35083=CARTESIAN_POINT('Ctrl Pts',(-40.3171916921862,47.2362996694757,-456.743217132386));
#35084=CARTESIAN_POINT('Ctrl Pts',(-40.5195236792124,47.4136404438748,-456.456792590743));
#35085=CARTESIAN_POINT('Ctrl Pts',(-40.7212794045083,47.5913518598966,-456.170245768125));
#35086=CARTESIAN_POINT('Ctrl Pts',(-40.9181659593801,47.7647743905864,-455.890614463328));
#35087=CARTESIAN_POINT('Ctrl Pts',(-41.1143879832752,47.9387398116063,-455.610863743241));
#35088=CARTESIAN_POINT('Ctrl Pts',(-41.3098930235588,48.1132901226562,-455.330988558208));
#35089=CARTESIAN_POINT('Ctrl Pts',(-41.5616503838927,48.3380634865121,-454.970585380343));
#35090=CARTESIAN_POINT('Ctrl Pts',(-41.8121923904017,48.5638380597795,-454.60997068752));
#35091=CARTESIAN_POINT('Ctrl Pts',(-42.0619290902754,48.7902603788824,-454.249233490737));
#35092=CARTESIAN_POINT('Ctrl Pts',(-42.6414812933395,49.3157079960141,-453.412087659836));
#35093=CARTESIAN_POINT('Ctrl Pts',(-43.2168880235552,49.8444141500828,-452.574318560928));
#35094=CARTESIAN_POINT('Ctrl Pts',(-43.7934308880573,50.3717913051393,-451.737082281518));
#35095=CARTESIAN_POINT('Ctrl Pts',(-44.1402842673473,50.6890661508696,-451.233393396167));
#35096=CARTESIAN_POINT('Ctrl Pts',(-44.4877284502663,51.005671883583,-450.729933812533));
#35097=CARTESIAN_POINT('Ctrl Pts',(-44.835455089325,51.3219052879597,-450.226622807157));
#35098=CARTESIAN_POINT('Ctrl Pts',(-45.3127104949056,51.7559361751894,-449.535827593268));
#35099=CARTESIAN_POINT('Ctrl Pts',(-45.7904378177086,52.1893383421085,-448.845299007264));
#35100=CARTESIAN_POINT('Ctrl Pts',(-46.2679227237807,52.622775348591,-448.154844964195));
#35101=CARTESIAN_POINT('Ctrl Pts',(-46.2683832524782,52.6231933935963,-448.154179029215));
#35102=CARTESIAN_POINT('Ctrl Pts',(-46.2688437807351,52.623611438893,-448.153513094256));
#35103=CARTESIAN_POINT('Ctrl Pts',(-46.2693043085481,52.6240294844856,-448.152847159317));
#35104=CARTESIAN_POINT('Ctrl Pts',(-46.2873779222567,52.640435865038,-448.126712253849));
#35105=CARTESIAN_POINT('Ctrl Pts',(-46.3054508392597,52.656842716909,-448.100577375332));
#35106=CARTESIAN_POINT('Ctrl Pts',(-46.3235228985128,52.673250241708,-448.074442481881));
#35107=CARTESIAN_POINT('Ctrl Pts',(-46.3459982461223,52.6936554881774,-448.041939776636));
#35108=CARTESIAN_POINT('Ctrl Pts',(-46.3684721674282,52.7140618959818,-448.009437025237));
#35109=CARTESIAN_POINT('Ctrl Pts',(-46.3909453552282,52.7344686413403,-447.976934377398));
#35110=CARTESIAN_POINT('Ctrl Pts',(-47.1702843467058,53.4421462742838,-446.849787618707));
#35111=CARTESIAN_POINT('Ctrl Pts',(-47.9488861626814,54.1500539505149,-445.722799052326));
#35112=CARTESIAN_POINT('Ctrl Pts',(-48.7276050737667,54.857706910967,-444.595804874112));
#35113=CARTESIAN_POINT('Ctrl Pts',(-48.7315358189299,54.8612789360096,-444.590116137326));
#35114=CARTESIAN_POINT('Ctrl Pts',(-48.7354665673788,54.8648509542079,-444.584427400473));
#35115=CARTESIAN_POINT('Ctrl Pts',(-48.7393973192287,54.8684229654936,-444.578738663531));
#35116=CARTESIAN_POINT('Ctrl Pts',(-48.7399674832552,54.8689410934282,-444.577913499979));
#35117=CARTESIAN_POINT('Ctrl Pts',(-48.7405376473532,54.8694592212174,-444.577088336424));
#35118=CARTESIAN_POINT('Ctrl Pts',(-48.7413170873395,54.8701675249388,-444.575960300843));
#35119=CARTESIAN_POINT('Ctrl Pts',(-48.7415263631654,54.8703577009971,-444.575657428817));
#35120=CARTESIAN_POINT('Ctrl Pts',(-49.5628865989681,55.6167555612587,-443.386953354745));
#35121=CARTESIAN_POINT('Ctrl Pts',(-50.3841865870562,56.3626616466884,-442.198548263877));
#35122=CARTESIAN_POINT('Ctrl Pts',(-51.207704839932,57.1111550019579,-441.006781019456));
#35123=CARTESIAN_POINT('Ctrl Pts',(-51.2099532458194,57.1131985758379,-441.003527202775));
#35124=CARTESIAN_POINT('Ctrl Pts',(-51.261754652298,57.1602809218721,-440.928561939201));
#35125=CARTESIAN_POINT('Ctrl Pts',(-51.3113076531195,57.2053196899347,-440.856850493122));
#35126=CARTESIAN_POINT('Ctrl Pts',(-51.360860653941,57.2503584579972,-440.785139047043));
#35127=CARTESIAN_POINT('Ctrl Pts',(-35.9475629882934,43.8519642786695,-462.499999999992));
#35128=CARTESIAN_POINT('Ctrl Pts',(-36.7954828795889,44.5884643863239,-461.305833776046));
#35129=CARTESIAN_POINT('Ctrl Pts',(-37.6475601780025,45.322293983457,-460.112495563219));
#35130=CARTESIAN_POINT('Ctrl Pts',(-38.4912669551212,46.0623537625501,-458.917387277545));
#35131=CARTESIAN_POINT('Ctrl Pts',(-38.5267721915119,46.0934972807872,-458.867094209685));
#35132=CARTESIAN_POINT('Ctrl Pts',(-38.5622626071291,46.1246518317674,-458.816798008153));
#35133=CARTESIAN_POINT('Ctrl Pts',(-38.5977380083514,46.155817499324,-458.766498650856));
#35134=CARTESIAN_POINT('Ctrl Pts',(-39.0060055809331,46.5144866335072,-458.187630032083));
#35135=CARTESIAN_POINT('Ctrl Pts',(-39.4122841582898,46.8746279159974,-457.608343242923));
#35136=CARTESIAN_POINT('Ctrl Pts',(-39.8162772669613,47.2363679985138,-457.028603802983));
#35137=CARTESIAN_POINT('Ctrl Pts',(-40.0158065575446,47.4150288233912,-456.742274663472));
#35138=CARTESIAN_POINT('Ctrl Pts',(-40.214607115487,47.5943656169502,-456.455832427307));
#35139=CARTESIAN_POINT('Ctrl Pts',(-40.4128162635484,47.7741101699194,-456.169277473623));
#35140=CARTESIAN_POINT('Ctrl Pts',(-40.6062418342412,47.9495167698522,-455.889638233994));
#35141=CARTESIAN_POINT('Ctrl Pts',(-40.7990596571074,48.1253847665991,-455.609890510788));
#35142=CARTESIAN_POINT('Ctrl Pts',(-40.9912307836365,48.3017409579112,-455.330031412169));
#35143=CARTESIAN_POINT('Ctrl Pts',(-41.2386949690977,48.5288398047689,-454.969648949234));
#35144=CARTESIAN_POINT('Ctrl Pts',(-41.4850766216601,48.7567602390532,-454.609079830539));
#35145=CARTESIAN_POINT('Ctrl Pts',(-41.7307438807284,48.9852135040821,-454.248403823038));
#35146=CARTESIAN_POINT('Ctrl Pts',(-42.3008523240842,49.5153742418177,-453.411399991223));
#35147=CARTESIAN_POINT('Ctrl Pts',(-42.8671875079075,50.0483157782754,-452.573834627159));
#35148=CARTESIAN_POINT('Ctrl Pts',(-43.4344073031703,50.5803663332472,-451.736720752602));
#35149=CARTESIAN_POINT('Ctrl Pts',(-43.775651840048,50.9004527384523,-451.233105507114));
#35150=CARTESIAN_POINT('Ctrl Pts',(-44.1173979239211,51.2200133360429,-450.729690683017));
#35151=CARTESIAN_POINT('Ctrl Pts',(-44.4593743560895,51.5392863902607,-450.226406067365));
#35152=CARTESIAN_POINT('Ctrl Pts',(-44.9287375928996,51.977489202085,-449.535647073417));
#35153=CARTESIAN_POINT('Ctrl Pts',(-45.3985115831802,52.4151783217421,-448.845128256085));
#35154=CARTESIAN_POINT('Ctrl Pts',(-45.8680276737047,52.8529293881298,-448.154674598474));
#35155=CARTESIAN_POINT('Ctrl Pts',(-45.8684805165712,52.8533515939961,-448.154008663867));
#35156=CARTESIAN_POINT('Ctrl Pts',(-45.8689333591152,52.8537738000197,-448.153342729301));
#35157=CARTESIAN_POINT('Ctrl Pts',(-45.8693862013353,52.8541960062022,-448.152676794776));
#35158=CARTESIAN_POINT('Ctrl Pts',(-45.8871581906202,52.8707656709084,-448.126541905606));
#35159=CARTESIAN_POINT('Ctrl Pts',(-45.9049296761791,52.8873355863782,-448.100407079054));
#35160=CARTESIAN_POINT('Ctrl Pts',(-45.9227006019857,52.9039058265311,-448.07427229799));
#35161=CARTESIAN_POINT('Ctrl Pts',(-45.9448014444662,52.9245134342308,-448.041769732515));
#35162=CARTESIAN_POINT('Ctrl Pts',(-45.9669013828508,52.9451215904905,-448.00926722852));
#35163=CARTESIAN_POINT('Ctrl Pts',(-45.9890006951563,52.9657299712847,-447.976764841665));
#35164=CARTESIAN_POINT('Ctrl Pts',(-46.7553742029008,53.6804000415537,-446.84962713344));
#35165=CARTESIAN_POINT('Ctrl Pts',(-47.5210506383138,54.395272382088,-445.72264325122));
#35166=CARTESIAN_POINT('Ctrl Pts',(-48.2868348910593,55.1098674340124,-444.595668641787));
#35167=CARTESIAN_POINT('Ctrl Pts',(-48.2907003458527,55.1134745007011,-444.589980003779));
#35168=CARTESIAN_POINT('Ctrl Pts',(-48.2945658035078,55.1170815601898,-444.584291366036));
#35169=CARTESIAN_POINT('Ctrl Pts',(-48.2984312641301,55.1206886124145,-444.57860272854));
#35170=CARTESIAN_POINT('Ctrl Pts',(-48.2989919575233,55.1212118231128,-444.577777579412));
#35171=CARTESIAN_POINT('Ctrl Pts',(-48.299552650979,55.1217350336583,-444.57695243029));
#35172=CARTESIAN_POINT('Ctrl Pts',(-48.30031914416,55.1224502857254,-444.575824414447));
#35173=CARTESIAN_POINT('Ctrl Pts',(-48.300524943831,55.1226423273794,-444.575521547722));
#35174=CARTESIAN_POINT('Ctrl Pts',(-49.1082420541422,55.8763622243326,-443.386838281281));
#35175=CARTESIAN_POINT('Ctrl Pts',(-49.9158834311692,56.6295730136096,-442.198468567746));
#35176=CARTESIAN_POINT('Ctrl Pts',(-50.7256539365221,57.3853557303075,-441.006801374657));
#35177=CARTESIAN_POINT('Ctrl Pts',(-50.7278648073123,57.3874192056623,-441.003547831624));
#35178=CARTESIAN_POINT('Ctrl Pts',(-50.7788014272818,57.434960059129,-440.928588883822));
#35179=CARTESIAN_POINT('Ctrl Pts',(-50.8275271770784,57.4804374334134,-440.856883479385));
#35180=CARTESIAN_POINT('Ctrl Pts',(-50.876252926875,57.5259148076979,-440.785178074948));
#35181=CARTESIAN_POINT('Ctrl Pts',(-35.7167344653798,43.9786237267065,-462.499999999992));
#35182=CARTESIAN_POINT('Ctrl Pts',(-36.5492153513124,44.7241607642468,-461.305609373832));
#35183=CARTESIAN_POINT('Ctrl Pts',(-37.385971991095,45.4667569183785,-460.112099964991));
#35184=CARTESIAN_POINT('Ctrl Pts',(-38.2141497530743,46.2157296786755,-458.916847466227));
#35185=CARTESIAN_POINT('Ctrl Pts',(-38.2490014906803,46.247248276873,-458.86654832953));
#35186=CARTESIAN_POINT('Ctrl Pts',(-38.2838380373636,46.2787781663597,-458.816246106305));
#35187=CARTESIAN_POINT('Ctrl Pts',(-38.3186592191928,46.3103194452406,-458.765940786591));
#35188=CARTESIAN_POINT('Ctrl Pts',(-38.7193977278485,46.6733112908902,-458.187003549521));
#35189=CARTESIAN_POINT('Ctrl Pts',(-39.118101195542,47.0378116345601,-457.607656189956));
#35190=CARTESIAN_POINT('Ctrl Pts',(-39.5145047963644,47.4039698112403,-457.02788357782));
#35191=CARTESIAN_POINT('Ctrl Pts',(-39.7102856836097,47.5848127010472,-456.7415380548));
#35192=CARTESIAN_POINT('Ctrl Pts',(-39.9055055724271,47.7660599804359,-456.455088801439));
#35193=CARTESIAN_POINT('Ctrl Pts',(-40.1001326109166,47.9477296040555,-456.168534004658));
#35194=CARTESIAN_POINT('Ctrl Pts',(-40.2900625226301,48.1250148150051,-455.888894918146));
#35195=CARTESIAN_POINT('Ctrl Pts',(-40.4794278543523,48.302702230494,-455.609155321109));
#35196=CARTESIAN_POINT('Ctrl Pts',(-40.6681990411052,48.480808511884,-455.329313535));
#35197=CARTESIAN_POINT('Ctrl Pts',(-40.9112850281215,48.7101609991476,-454.968953365873));
#35198=CARTESIAN_POINT('Ctrl Pts',(-41.1533858001681,48.9402080524733,-454.608423746657));
#35199=CARTESIAN_POINT('Ctrl Pts',(-41.3948452851314,49.1707000470535,-454.24779837114));
#35200=CARTESIAN_POINT('Ctrl Pts',(-41.9551889452019,49.7055919684858,-453.410912038584));
#35201=CARTESIAN_POINT('Ctrl Pts',(-42.5120796284979,50.2428796389268,-452.573510142326));
#35202=CARTESIAN_POINT('Ctrl Pts',(-43.0698100792138,50.7794473054458,-451.736512580054));
#35203=CARTESIAN_POINT('Ctrl Pts',(-43.4053457409566,51.1022512456362,-451.232967309084));
#35204=CARTESIAN_POINT('Ctrl Pts',(-43.7413162638231,51.4246393226488,-450.729595690695));
#35205=CARTESIAN_POINT('Ctrl Pts',(-44.0774759502298,51.7468086495426,-450.226336299815));
#35206=CARTESIAN_POINT('Ctrl Pts',(-44.5388556935541,52.1889866005578,-449.535611926908));
#35207=CARTESIAN_POINT('Ctrl Pts',(-45.0005917476346,52.6307524990785,-448.845098958398));
#35208=CARTESIAN_POINT('Ctrl Pts',(-45.4620498885854,53.0726152328005,-448.154638776746));
#35209=CARTESIAN_POINT('Ctrl Pts',(-45.4624949596523,53.0730414043226,-448.153972835846));
#35210=CARTESIAN_POINT('Ctrl Pts',(-45.4629400304607,53.0734675759348,-448.153306894995));
#35211=CARTESIAN_POINT('Ctrl Pts',(-45.4633851010109,53.0738937476368,-448.152640954193));
#35212=CARTESIAN_POINT('Ctrl Pts',(-45.4808520877385,53.0906190408758,-448.126505818669));
#35213=CARTESIAN_POINT('Ctrl Pts',(-45.4983186766536,53.1073444726047,-448.100370758764));
#35214=CARTESIAN_POINT('Ctrl Pts',(-45.515784877734,53.1240700362378,-448.074235773136));
#35215=CARTESIAN_POINT('Ctrl Pts',(-45.5375067487839,53.1448708122511,-448.041732953258));
#35216=CARTESIAN_POINT('Ctrl Pts',(-45.5592280199817,53.1656717922767,-448.009230248262));
#35217=CARTESIAN_POINT('Ctrl Pts',(-45.5809487105189,53.1864729636486,-447.976727655573));
#35218=CARTESIAN_POINT('Ctrl Pts',(-46.3341921403375,53.9078287438245,-446.849582809351));
#35219=CARTESIAN_POINT('Ctrl Pts',(-47.086737395337,54.6294145238461,-445.722573035568));
#35220=CARTESIAN_POINT('Ctrl Pts',(-47.8393839597814,55.3507028414842,-444.595590722938));
#35221=CARTESIAN_POINT('Ctrl Pts',(-47.8431830993691,55.3543436938193,-444.589902046046));
#35222=CARTESIAN_POINT('Ctrl Pts',(-47.8469822415353,55.3579845385777,-444.584213369854));
#35223=CARTESIAN_POINT('Ctrl Pts',(-47.8507813863828,55.3616253756915,-444.578524694348));
#35224=CARTESIAN_POINT('Ctrl Pts',(-47.85133246053,55.3621534869608,-444.577699539707));
#35225=CARTESIAN_POINT('Ctrl Pts',(-47.8518835347336,55.3626815980692,-444.57687438508));
#35226=CARTESIAN_POINT('Ctrl Pts',(-47.8526368779575,55.3634035494146,-444.575746361725));
#35227=CARTESIAN_POINT('Ctrl Pts',(-47.8528391469287,55.363597389791,-444.575443492985));
#35228=CARTESIAN_POINT('Ctrl Pts',(-48.6466990572118,56.1243768599733,-443.386752320462));
#35229=CARTESIAN_POINT('Ctrl Pts',(-49.4404742924094,56.884628672487,-442.198393858917));
#35230=CARTESIAN_POINT('Ctrl Pts',(-50.2363376755567,57.6473823416216,-441.00681768439));
#35231=CARTESIAN_POINT('Ctrl Pts',(-50.2385105764817,57.6494648487129,-441.003564390457));
#35232=CARTESIAN_POINT('Ctrl Pts',(-50.2885724016608,57.6974441622301,-440.928611195469));
#35233=CARTESIAN_POINT('Ctrl Pts',(-50.336461326554,57.7433409654976,-440.856911294148));
#35234=CARTESIAN_POINT('Ctrl Pts',(-50.3843502514473,57.7892377687651,-440.785211392827));
#35235=CARTESIAN_POINT('Ctrl Pts',(-35.4827207341128,44.0991249603451,-462.499999999992));
#35236=CARTESIAN_POINT('Ctrl Pts',(-36.2994515423613,44.8532246984928,-461.305379862298));
#35237=CARTESIAN_POINT('Ctrl Pts',(-37.1204817421049,45.6042217030189,-460.111741809773));
#35238=CARTESIAN_POINT('Ctrl Pts',(-37.9331529959546,46.3612892574823,-458.916436947675));
#35239=CARTESIAN_POINT('Ctrl Pts',(-37.9673521819257,46.3931485043366,-458.866135607401));
#35240=CARTESIAN_POINT('Ctrl Pts',(-38.0015365664587,46.4250185004757,-458.815831315687));
#35241=CARTESIAN_POINT('Ctrl Pts',(-38.0357059902503,46.4568993332573,-458.765524060738));
#35242=CARTESIAN_POINT('Ctrl Pts',(-38.4289437614191,46.8237989246134,-458.186564552082));
#35243=CARTESIAN_POINT('Ctrl Pts',(-38.8202000143432,47.1921338048814,-457.607212569856));
#35244=CARTESIAN_POINT('Ctrl Pts',(-39.2092322209606,47.5620369281162,-457.027450190993));
#35245=CARTESIAN_POINT('Ctrl Pts',(-39.4013724296281,47.7447294200904,-456.741109722113));
#35246=CARTESIAN_POINT('Ctrl Pts',(-39.5929701347858,47.9278044479374,-456.454669146702));
#35247=CARTESIAN_POINT('Ctrl Pts',(-39.7839961708745,48.1112779928082,-456.168126315193));
#35248=CARTESIAN_POINT('Ctrl Pts',(-39.9704119867388,48.2903235891937,-455.888498905184));
#35249=CARTESIAN_POINT('Ctrl Pts',(-40.1562833938311,48.4697486991241,-455.608774115215));
#35250=CARTESIAN_POINT('Ctrl Pts',(-40.3415833236734,48.6495681499273,-455.328949954032));
#35251=CARTESIAN_POINT('Ctrl Pts',(-40.5801992751574,48.8811267338146,-454.968612481019));
#35252=CARTESIAN_POINT('Ctrl Pts',(-40.8178676002812,49.1133392152827,-454.608110230613));
#35253=CARTESIAN_POINT('Ctrl Pts',(-41.0549375578775,49.3459520531875,-454.247516228856));
#35254=CARTESIAN_POINT('Ctrl Pts',(-41.605094648424,49.8857657158846,-453.410702703908));
#35255=CARTESIAN_POINT('Ctrl Pts',(-42.1520299024585,50.4277350191744,-452.573395183637));
#35256=CARTESIAN_POINT('Ctrl Pts',(-42.700102688811,50.9686952648692,-451.736505220437));
#35257=CARTESIAN_POINT('Ctrl Pts',(-43.0298282127016,51.2941418202487,-451.233024682037));
#35258=CARTESIAN_POINT('Ctrl Pts',(-43.3599651617063,51.6192234296391,-450.729695153505));
#35259=CARTESIAN_POINT('Ctrl Pts',(-43.6902720539313,51.9441260974159,-450.226460975302));
#35260=CARTESIAN_POINT('Ctrl Pts',(-44.1436188272522,52.3900555634583,-449.535771206835));
#35261=CARTESIAN_POINT('Ctrl Pts',(-44.5972857048412,52.835647966713,-448.845261050184));
#35262=CARTESIAN_POINT('Ctrl Pts',(-45.0506493623309,53.2813834737626,-448.154786794391));
#35263=CARTESIAN_POINT('Ctrl Pts',(-45.0510866263617,53.2818133805301,-448.154120839917));
#35264=CARTESIAN_POINT('Ctrl Pts',(-45.0515238901104,53.2822432874305,-448.153454885476));
#35265=CARTESIAN_POINT('Ctrl Pts',(-45.0519611535773,53.2826731944639,-448.152788931068));
#35266=CARTESIAN_POINT('Ctrl Pts',(-45.0691217479385,53.2995450824021,-448.126653261581));
#35267=CARTESIAN_POINT('Ctrl Pts',(-45.0862819082435,53.3164171750821,-448.100517643539));
#35268=CARTESIAN_POINT('Ctrl Pts',(-45.1034416450612,53.3332894643605,-448.07438207641));
#35269=CARTESIAN_POINT('Ctrl Pts',(-45.1247823813031,53.3542727159754,-448.041878533347));
#35270=CARTESIAN_POINT('Ctrl Pts',(-45.1461224625502,53.3752562716634,-448.00937506903));
#35271=CARTESIAN_POINT('Ctrl Pts',(-45.1674619091309,53.3962401157622,-447.976871682436));
#35272=CARTESIAN_POINT('Ctrl Pts',(-45.9074843271741,54.1239307328129,-446.849699304724));
#35273=CARTESIAN_POINT('Ctrl Pts',(-46.6467436227848,54.8519680802525,-445.722620410717));
#35274=CARTESIAN_POINT('Ctrl Pts',(-47.3860866986765,55.5796997443964,-444.595592240322));
#35275=CARTESIAN_POINT('Ctrl Pts',(-47.3898186861473,55.583373120859,-444.589903331954));
#35276=CARTESIAN_POINT('Ctrl Pts',(-47.3935506757501,55.5870464895352,-444.584214424878));
#35277=CARTESIAN_POINT('Ctrl Pts',(-47.3972826675936,55.5907198503415,-444.578525519089));
#35278=CARTESIAN_POINT('Ctrl Pts',(-47.3978240010529,55.5912526792425,-444.577700331045));
#35279=CARTESIAN_POINT('Ctrl Pts',(-47.3983653345593,55.591785507978,-444.576875143028));
#35280=CARTESIAN_POINT('Ctrl Pts',(-47.3991053618007,55.5925139085243,-444.575747074044));
#35281=CARTESIAN_POINT('Ctrl Pts',(-47.3993040554946,55.5927094804788,-444.575444193054));
#35282=CARTESIAN_POINT('Ctrl Pts',(-48.1791318076515,56.3602850002595,-443.386704951096));
#35283=CARTESIAN_POINT('Ctrl Pts',(-48.9588592874826,57.127321149212,-442.198324735079));
#35284=CARTESIAN_POINT('Ctrl Pts',(-49.7406729832468,57.8967208089775,-441.006829369427));
#35285=CARTESIAN_POINT('Ctrl Pts',(-49.7428075253643,57.8988214600748,-441.003576296889));
#35286=CARTESIAN_POINT('Ctrl Pts',(-49.7919856016638,57.9472187693854,-440.928628220373));
#35287=CARTESIAN_POINT('Ctrl Pts',(-49.8390291362108,57.9935154256164,-440.856933215362));
#35288=CARTESIAN_POINT('Ctrl Pts',(-49.8860726707578,58.0398120818473,-440.785238210351));
#35289=CARTESIAN_POINT('Ctrl Pts',(-35.0926443215359,44.2999879125929,-462.499999999992));
#35290=CARTESIAN_POINT('Ctrl Pts',(-35.8831213977166,45.0683607770092,-461.304997290577));
#35291=CARTESIAN_POINT('Ctrl Pts',(-36.6779372668746,45.8333611204278,-460.111144802486));
#35292=CARTESIAN_POINT('Ctrl Pts',(-37.4647607936271,46.6039218500648,-458.915752656189));
#35293=CARTESIAN_POINT('Ctrl Pts',(-37.4978722442788,46.6363489225989,-458.865447642783));
#35294=CARTESIAN_POINT('Ctrl Pts',(-37.5309695427217,46.6687858409527,-458.815139903113));
#35295=CARTESIAN_POINT('Ctrl Pts',(-37.5640525540381,46.7012326745701,-458.764829422331));
#35296=CARTESIAN_POINT('Ctrl Pts',(-37.9447873803808,47.0746460692748,-458.185832789269));
#35297=CARTESIAN_POINT('Ctrl Pts',(-38.3236299052502,47.4493727209661,-457.606473101551));
#35298=CARTESIAN_POINT('Ctrl Pts',(-38.7003747687633,47.8255182783924,-457.026727780484));
#35299=CARTESIAN_POINT('Ctrl Pts',(-38.8864463470506,48.0112938637139,-456.740395736327));
#35300=CARTESIAN_POINT('Ctrl Pts',(-39.0720062509222,48.1974155570617,-456.45396962615));
#35301=CARTESIAN_POINT('Ctrl Pts',(-39.2570297926673,48.3838960499711,-456.167446739499));
#35302=CARTESIAN_POINT('Ctrl Pts',(-39.4375879783198,48.5658760247446,-455.887838792999));
#35303=CARTESIAN_POINT('Ctrl Pts',(-39.6176353785126,48.7481976895492,-455.608138684863));
#35304=CARTESIAN_POINT('Ctrl Pts',(-39.7971490861727,48.9308728145696,-455.328343902587));
#35305=CARTESIAN_POINT('Ctrl Pts',(-40.0283139559821,49.1661087307745,-454.968044261623));
#35306=CARTESIAN_POINT('Ctrl Pts',(-40.2585938557126,49.4019307544559,-454.607587632161));
#35307=CARTESIAN_POINT('Ctrl Pts',(-40.4883469303252,49.6380788163462,-454.24704592718));
#35308=CARTESIAN_POINT('Ctrl Pts',(-41.0215240749735,50.1860965069258,-453.410353764899));
#35309=CARTESIAN_POINT('Ctrl Pts',(-41.5518646697502,50.7358696024833,-452.573203559526));
#35310=CARTESIAN_POINT('Ctrl Pts',(-42.0838391397846,51.2841518182078,-451.736492952724));
#35311=CARTESIAN_POINT('Ctrl Pts',(-42.4038797716061,51.6140033366944,-451.233120316749));
#35312=CARTESIAN_POINT('Ctrl Pts',(-42.7242927631654,51.9435747828198,-450.729860947609));
#35313=CARTESIAN_POINT('Ctrl Pts',(-43.0448436596819,52.2730336439458,-450.226668796296));
#35314=CARTESIAN_POINT('Ctrl Pts',(-43.4848003122421,52.725216493136,-449.53603670981));
#35315=CARTESIAN_POINT('Ctrl Pts',(-43.9250167166423,53.1771872795364,-448.845531240238));
#35316=CARTESIAN_POINT('Ctrl Pts',(-44.3648877168719,53.6293782946376,-448.155033524324));
#35317=CARTESIAN_POINT('Ctrl Pts',(-44.3653119673901,53.6298144276682,-448.154367547222));
#35318=CARTESIAN_POINT('Ctrl Pts',(-44.3657362175869,53.6302505609037,-448.153701570128));
#35319=CARTESIAN_POINT('Ctrl Pts',(-44.3661604674627,53.6306866943438,-448.153035593041));
#35320=CARTESIAN_POINT('Ctrl Pts',(-44.3828103377971,53.6478029403118,-448.126899033492));
#35321=CARTESIAN_POINT('Ctrl Pts',(-44.3994597136609,53.6649195014566,-448.100762485096));
#35322=CARTESIAN_POINT('Ctrl Pts',(-44.4161086066083,53.6820363670388,-448.074625948665));
#35323=CARTESIAN_POINT('Ctrl Pts',(-44.4368140309913,53.7033237863947,-448.042121200129));
#35324=CARTESIAN_POINT('Ctrl Pts',(-44.4575187084622,53.7246116766146,-448.009616470102));
#35325=CARTESIAN_POINT('Ctrl Pts',(-44.478222661245,53.7459000170419,-447.977111760154));
#35326=CARTESIAN_POINT('Ctrl Pts',(-45.1962070355543,54.4841501445497,-446.849893490325));
#35327=CARTESIAN_POINT('Ctrl Pts',(-45.913320026553,55.2229415800519,-445.722699380136));
#35328=CARTESIAN_POINT('Ctrl Pts',(-46.6304875785502,55.9614136288578,-444.595594769643));
#35329=CARTESIAN_POINT('Ctrl Pts',(-46.6341076304664,55.9651412196388,-444.589905475428));
#35330=CARTESIAN_POINT('Ctrl Pts',(-46.6377276837699,55.9688688022845,-444.584216183493));
#35331=CARTESIAN_POINT('Ctrl Pts',(-46.6413477385799,55.9725963766842,-444.578526893846));
#35332=CARTESIAN_POINT('Ctrl Pts',(-46.6418728353313,55.9731370693837,-444.577701650123));
#35333=CARTESIAN_POINT('Ctrl Pts',(-46.6423979321143,55.9736777619098,-444.576876406447));
#35334=CARTESIAN_POINT('Ctrl Pts',(-46.6431157630056,55.9744169125997,-444.575748261405));
#35335=CARTESIAN_POINT('Ctrl Pts',(-46.6433084970863,55.974615370914,-444.575445359997));
#35336=CARTESIAN_POINT('Ctrl Pts',(-47.3997461093869,56.7535191945194,-443.386625991318));
#35337=CARTESIAN_POINT('Ctrl Pts',(-48.1560574503936,57.5318641226853,-442.19820951287));
#35338=CARTESIAN_POINT('Ctrl Pts',(-48.9144517868643,58.312341953673,-441.006848847162));
#35339=CARTESIAN_POINT('Ctrl Pts',(-48.916522388862,58.3144728489302,-441.003596143665));
#35340=CARTESIAN_POINT('Ctrl Pts',(-48.9642273482186,58.3635669135128,-440.928656599108));
#35341=CARTESIAN_POINT('Ctrl Pts',(-49.0098617054858,58.4105300828157,-440.856969755731));
#35342=CARTESIAN_POINT('Ctrl Pts',(-49.0554960627529,58.4574932521186,-440.785282912355));
#35343=CARTESIAN_POINT('Ctrl Pts',(-34.6937162549713,44.4837348679316,-462.499999999992));
#35344=CARTESIAN_POINT('Ctrl Pts',(-35.4568775601461,45.2647808331932,-461.305006320268));
#35345=CARTESIAN_POINT('Ctrl Pts',(-36.2238622232575,46.0429432083199,-460.110949296857));
#35346=CARTESIAN_POINT('Ctrl Pts',(-36.9837888169173,46.8260011505549,-458.91546450044));
#35347=CARTESIAN_POINT('Ctrl Pts',(-37.0157683791055,46.8589541362374,-458.865155588091));
#35348=CARTESIAN_POINT('Ctrl Pts',(-37.0477354434537,46.8919157905208,-458.814844147584));
#35349=CARTESIAN_POINT('Ctrl Pts',(-37.0796898950869,46.9248861637916,-458.76453016749));
#35350=CARTESIAN_POINT('Ctrl Pts',(-37.4474367267489,47.3043246986239,-458.185493262703));
#35351=CARTESIAN_POINT('Ctrl Pts',(-37.8135129358142,47.6849180817468,-457.60611997644));
#35352=CARTESIAN_POINT('Ctrl Pts',(-38.1777442157752,48.066742731875,-457.026393048804));
#35353=CARTESIAN_POINT('Ctrl Pts',(-38.3576354251521,48.2553231802341,-456.74007008903));
#35354=CARTESIAN_POINT('Ctrl Pts',(-38.5370766294755,48.4442039585018,-456.453660871109));
#35355=CARTESIAN_POINT('Ctrl Pts',(-38.7160468882022,48.633394236783,-456.167163326133));
#35356=CARTESIAN_POINT('Ctrl Pts',(-38.8906978807008,48.8180185989985,-455.887580109712));
#35357=CARTESIAN_POINT('Ctrl Pts',(-39.064900390378,49.0029377005569,-455.607912779175));
#35358=CARTESIAN_POINT('Ctrl Pts',(-39.2386348864512,49.1881600800444,-455.328159397521));
#35359=CARTESIAN_POINT('Ctrl Pts',(-39.4623577023278,49.4266761677469,-454.967913069305));
#35360=CARTESIAN_POINT('Ctrl Pts',(-39.6853044481674,49.6656951536519,-454.607524049405));
#35361=CARTESIAN_POINT('Ctrl Pts',(-39.9077944947688,49.9049821886886,-454.247056749965));
#35362=CARTESIAN_POINT('Ctrl Pts',(-40.4241166722174,50.4602843464826,-453.410537257122));
#35363=CARTESIAN_POINT('Ctrl Pts',(-40.9379795370076,51.0170297897597,-452.573596243841));
#35364=CARTESIAN_POINT('Ctrl Pts',(-41.4533752294989,51.5722849505129,-451.737038725624));
#35365=CARTESIAN_POINT('Ctrl Pts',(-41.7634419194518,51.9063314555231,-451.233758189122));
#35366=CARTESIAN_POINT('Ctrl Pts',(-42.0738280092103,52.240150054641,-450.730566128798));
#35367=CARTESIAN_POINT('Ctrl Pts',(-42.3843277118328,52.573887105166,-450.227421760993));
#35368=CARTESIAN_POINT('Ctrl Pts',(-42.8104890836191,53.031941776608,-449.536855257452));
#35369=CARTESIAN_POINT('Ctrl Pts',(-43.2368704944582,53.4898406553964,-448.846379690617));
#35370=CARTESIAN_POINT('Ctrl Pts',(-43.662949213368,53.9479584646017,-448.155891290016));
#35371=CARTESIAN_POINT('Ctrl Pts',(-43.6633601613895,53.9484003139571,-448.155225321899));
#35372=CARTESIAN_POINT('Ctrl Pts',(-43.6637711091287,53.9488421635163,-448.15455935377));
#35373=CARTESIAN_POINT('Ctrl Pts',(-43.664182056586,53.9492840132792,-448.153893385629));
#35374=CARTESIAN_POINT('Ctrl Pts',(-43.6803098677362,53.9666245988145,-448.127757177169));
#35375=CARTESIAN_POINT('Ctrl Pts',(-43.6964372445572,53.9839654980612,-448.101620950182));
#35376=CARTESIAN_POINT('Ctrl Pts',(-43.7125641962304,54.0013067017012,-448.07548470511));
#35377=CARTESIAN_POINT('Ctrl Pts',(-43.7326205074486,54.0228731194691,-448.04298031892));
#35378=CARTESIAN_POINT('Ctrl Pts',(-43.7526761611034,54.0444400080328,-448.010475904759));
#35379=CARTESIAN_POINT('Ctrl Pts',(-43.7727311748529,54.0660073494699,-447.977971463475));
#35380=CARTESIAN_POINT('Ctrl Pts',(-44.4682112433112,54.8139328451354,-446.85076251054));
#35381=CARTESIAN_POINT('Ctrl Pts',(-45.1629219292152,55.5624028563398,-445.723520968408));
#35382=CARTESIAN_POINT('Ctrl Pts',(-45.857598497673,56.3106707131351,-444.596282029048));
#35383=CARTESIAN_POINT('Ctrl Pts',(-45.8611050216865,56.314447750288,-444.59059205678));
#35384=CARTESIAN_POINT('Ctrl Pts',(-45.8646115448271,56.3182247822925,-444.584902084578));
#35385=CARTESIAN_POINT('Ctrl Pts',(-45.8681180671893,56.3220018090526,-444.579212112446));
#35386=CARTESIAN_POINT('Ctrl Pts',(-45.8686266958145,56.3225496749236,-444.578386769726));
#35387=CARTESIAN_POINT('Ctrl Pts',(-45.8691353244232,56.3230975406842,-444.577561427008));
#35388=CARTESIAN_POINT('Ctrl Pts',(-45.8698306425161,56.3238464975938,-444.576433146507));
#35389=CARTESIAN_POINT('Ctrl Pts',(-45.8700173320142,56.3240475888386,-444.576130208722));
#35390=CARTESIAN_POINT('Ctrl Pts',(-46.6027313019823,57.1132851013013,-443.387168045725));
#35391=CARTESIAN_POINT('Ctrl Pts',(-47.3352250969972,57.9020921615662,-442.198511933312));
#35392=CARTESIAN_POINT('Ctrl Pts',(-48.0699634411771,58.6930115612169,-441.006849591051));
#35393=CARTESIAN_POINT('Ctrl Pts',(-48.0719694582289,58.695170964141,-441.003596063446));
#35394=CARTESIAN_POINT('Ctrl Pts',(-48.1181864730666,58.7449218132285,-440.928637521526));
#35395=CARTESIAN_POINT('Ctrl Pts',(-48.1623974690588,58.792513259741,-440.856932505353));
#35396=CARTESIAN_POINT('Ctrl Pts',(-48.2066084650511,58.8401047062535,-440.785227489179));
#35397=CARTESIAN_POINT('Ctrl Pts',(-34.2872595209354,44.6497527723323,-462.499999999992));
#35398=CARTESIAN_POINT('Ctrl Pts',(-35.0224304000914,45.4421310218592,-461.305151339373));
#35399=CARTESIAN_POINT('Ctrl Pts',(-35.7607385756046,46.2323164757708,-460.110931894838));
#35400=CARTESIAN_POINT('Ctrl Pts',(-36.4931193505426,47.0266864032259,-458.915400919906));
#35401=CARTESIAN_POINT('Ctrl Pts',(-36.5239397175793,47.0601154248016,-458.865090064252));
#35402=CARTESIAN_POINT('Ctrl Pts',(-36.5547495888943,47.0935518558537,-458.814776886249));
#35403=CARTESIAN_POINT('Ctrl Pts',(-36.5855488679042,47.1269957313529,-458.764461378322));
#35404=CARTESIAN_POINT('Ctrl Pts',(-36.9400014306773,47.5118835521334,-458.185406890509));
#35405=CARTESIAN_POINT('Ctrl Pts',(-37.2930508462519,47.8977574574093,-457.606043765974));
#35406=CARTESIAN_POINT('Ctrl Pts',(-37.6445513595258,48.2846701266294,-457.026360754561));
#35407=CARTESIAN_POINT('Ctrl Pts',(-37.8181549348041,48.4757635110216,-456.740059484693));
#35408=CARTESIAN_POINT('Ctrl Pts',(-37.9913807419683,48.6671102582059,-456.45368019583));
#35409=CARTESIAN_POINT('Ctrl Pts',(-38.1642112882018,48.8587166783817,-456.1672215441));
#35410=CARTESIAN_POINT('Ctrl Pts',(-38.3328707439603,49.0456988713503,-455.887676282276));
#35411=CARTESIAN_POINT('Ctrl Pts',(-38.5011537998596,49.2329283499863,-455.608055444416));
#35412=CARTESIAN_POINT('Ctrl Pts',(-38.6690439880478,49.4204110496045,-455.328357739766));
#35413=CARTESIAN_POINT('Ctrl Pts',(-38.8852409236505,49.6618378153579,-454.968183108402));
#35414=CARTESIAN_POINT('Ctrl Pts',(-39.1007863839428,49.9036844796046,-454.607881012199));
#35415=CARTESIAN_POINT('Ctrl Pts',(-39.3159450882721,50.1457533784629,-454.247505626363));
#35416=CARTESIAN_POINT('Ctrl Pts',(-39.8152537648325,50.7075112766714,-453.411199433092));
#35417=CARTESIAN_POINT('Ctrl Pts',(-40.3124792433739,51.2704659645045,-452.574498490218));
#35418=CARTESIAN_POINT('Ctrl Pts',(-40.8109390344613,51.8321453062596,-451.738081361453));
#35419=CARTESIAN_POINT('Ctrl Pts',(-41.1108169336148,52.1700566564129,-451.234885284506));
#35420=CARTESIAN_POINT('Ctrl Pts',(-41.410962076571,52.5077819260265,-450.731753539923));
#35421=CARTESIAN_POINT('Ctrl Pts',(-41.711203404823,52.8454452232713,-450.228650126377));
#35422=CARTESIAN_POINT('Ctrl Pts',(-42.1232851402775,53.3088886750373,-449.538139832627));
#35423=CARTESIAN_POINT('Ctrl Pts',(-42.5355621332702,53.7722102900826,-448.84768546806));
#35424=CARTESIAN_POINT('Ctrl Pts',(-42.9476124941153,54.2357233582771,-448.157197595481));
#35425=CARTESIAN_POINT('Ctrl Pts',(-42.9480099119469,54.2361704112977,-448.156531627873));
#35426=CARTESIAN_POINT('Ctrl Pts',(-42.948407329566,54.2366174644969,-448.155865660234));
#35427=CARTESIAN_POINT('Ctrl Pts',(-42.9488047469729,54.2370645178746,-448.155199692564));
#35428=CARTESIAN_POINT('Ctrl Pts',(-42.9644015654331,54.2546093215285,-448.129063502567));
#35429=CARTESIAN_POINT('Ctrl Pts',(-42.9799980571234,54.2721544000718,-448.102927264174));
#35430=CARTESIAN_POINT('Ctrl Pts',(-42.9955942275873,54.2896997469008,-448.076790977015));
#35431=CARTESIAN_POINT('Ctrl Pts',(-43.0149904318407,54.3115200476971,-448.044286538483));
#35432=CARTESIAN_POINT('Ctrl Pts',(-43.0343861392631,54.3333407634428,-448.011782024527));
#35433=CARTESIAN_POINT('Ctrl Pts',(-43.0537813605145,54.3551618814368,-447.979277434437));
#35434=CARTESIAN_POINT('Ctrl Pts',(-43.7263807400131,55.1118879962072,-446.852063321111));
#35435=CARTESIAN_POINT('Ctrl Pts',(-44.3983956724348,55.8690977462486,-445.724757698917));
#35436=CARTESIAN_POINT('Ctrl Pts',(-45.0702692045423,56.6262622154341,-444.597330620593));
#35437=CARTESIAN_POINT('Ctrl Pts',(-45.0736606255018,56.6300841600827,-444.591639698654));
#35438=CARTESIAN_POINT('Ctrl Pts',(-45.0770520428539,56.6339061035798,-444.58594877362));
#35439=CARTESIAN_POINT('Ctrl Pts',(-45.0804434566555,56.6377280458573,-444.580257845486));
#35440=CARTESIAN_POINT('Ctrl Pts',(-45.0809353885358,56.638282426821,-444.579432364097));
#35441=CARTESIAN_POINT('Ctrl Pts',(-45.0814273203415,56.6388368077588,-444.578606882642));
#35442=CARTESIAN_POINT('Ctrl Pts',(-45.0820998130759,56.6395946713239,-444.57747841239));
#35443=CARTESIAN_POINT('Ctrl Pts',(-45.0822803740693,56.6397981539734,-444.577175423649));
#35444=CARTESIAN_POINT('Ctrl Pts',(-45.7909413206515,57.4384214330053,-443.388013234218));
#35445=CARTESIAN_POINT('Ctrl Pts',(-46.4992668825881,58.2367877057615,-442.199018696807));
#35446=CARTESIAN_POINT('Ctrl Pts',(-47.2100390429521,59.0373060430022,-441.006896336889));
#35447=CARTESIAN_POINT('Ctrl Pts',(-47.2119796284694,59.0394916534735,-441.003641552419));
#35448=CARTESIAN_POINT('Ctrl Pts',(-47.2566892012544,59.0898463050323,-440.928654032679));
#35449=CARTESIAN_POINT('Ctrl Pts',(-47.2994581847153,59.1380153463707,-440.856921296449));
#35450=CARTESIAN_POINT('Ctrl Pts',(-47.3422271681762,59.1861843877091,-440.785188560218));
#35451=CARTESIAN_POINT('Ctrl Pts',(-34.2870189837742,44.6498510128264,-462.499999999991));
#35452=CARTESIAN_POINT('Ctrl Pts',(-35.022173298412,45.4422359681457,-461.30515142524));
#35453=CARTESIAN_POINT('Ctrl Pts',(-35.7604645033475,46.2324285367216,-460.110931884602));
#35454=CARTESIAN_POINT('Ctrl Pts',(-36.4928289768881,47.0268051580112,-458.915400882359));
#35455=CARTESIAN_POINT('Ctrl Pts',(-36.5236486579223,47.0602344612798,-458.865090025556));
#35456=CARTESIAN_POINT('Ctrl Pts',(-36.5544578444197,47.0936711732796,-458.814776846525));
#35457=CARTESIAN_POINT('Ctrl Pts',(-36.5852564398078,47.1271153289722,-458.764461337694));
#35458=CARTESIAN_POINT('Ctrl Pts',(-36.9397011351403,47.5120063743502,-458.185406839484));
#35459=CARTESIAN_POINT('Ctrl Pts',(-37.2927428415779,47.8978834043482,-457.606043720971));
#35460=CARTESIAN_POINT('Ctrl Pts',(-37.6442358209138,48.2847990843685,-457.026360735556));
#35461=CARTESIAN_POINT('Ctrl Pts',(-37.8178356752343,48.4758939557733,-456.740059478528));
#35462=CARTESIAN_POINT('Ctrl Pts',(-37.9910578041932,48.6672421621754,-456.453680207381));
#35463=CARTESIAN_POINT('Ctrl Pts',(-38.1638847170138,48.858850012082,-456.167221578672));
#35464=CARTESIAN_POINT('Ctrl Pts',(-38.3325406270483,49.0458336002762,-455.887676339314));
#35465=CARTESIAN_POINT('Ctrl Pts',(-38.5008201798844,49.2330644460553,-455.608055528972));
#35466=CARTESIAN_POINT('Ctrl Pts',(-38.6687069094829,49.4205484831939,-455.328357857276));
#35467=CARTESIAN_POINT('Ctrl Pts',(-38.884899391362,49.66197697131,-454.968183268347));
#35468=CARTESIAN_POINT('Ctrl Pts',(-39.1004404716694,49.9038253088016,-454.607881223591));
#35469=CARTESIAN_POINT('Ctrl Pts',(-39.3155948374051,50.1458958537967,-454.247505892154));
#35470=CARTESIAN_POINT('Ctrl Pts',(-39.8148934455952,50.7076575721175,-453.411199825125));
#35471=CARTESIAN_POINT('Ctrl Pts',(-40.3121090783446,51.2706159342137,-452.574499024332));
#35472=CARTESIAN_POINT('Ctrl Pts',(-40.8105588469142,51.8322990775026,-451.738081978642));
#35473=CARTESIAN_POINT('Ctrl Pts',(-41.1104307164308,52.170212714693,-451.234885951675));
#35474=CARTESIAN_POINT('Ctrl Pts',(-41.4105697988818,52.5079402960933,-450.731754242783));
#35475=CARTESIAN_POINT('Ctrl Pts',(-41.7108050563151,52.8456059167068,-450.22865085347));
#35476=CARTESIAN_POINT('Ctrl Pts',(-42.1228784595606,53.3090525573004,-449.538140592981));
#35477=CARTESIAN_POINT('Ctrl Pts',(-42.5351471056795,53.7723773812622,-448.847686240956));
#35478=CARTESIAN_POINT('Ctrl Pts',(-42.9471891646714,54.2358936421045,-448.157198368687));
#35479=CARTESIAN_POINT('Ctrl Pts',(-42.9475865744959,54.2363406982042,-448.15653240108));
#35480=CARTESIAN_POINT('Ctrl Pts',(-42.947983984108,54.2367877544828,-448.155866433441));
#35481=CARTESIAN_POINT('Ctrl Pts',(-42.948381393508,54.2372348109397,-448.155200465771));
#35482=CARTESIAN_POINT('Ctrl Pts',(-42.9639778977315,54.2547797354398,-448.129064275785));
#35483=CARTESIAN_POINT('Ctrl Pts',(-42.9795740752489,54.2723249348063,-448.102928037385));
#35484=CARTESIAN_POINT('Ctrl Pts',(-42.9951699316014,54.2898704024371,-448.076791750201));
#35485=CARTESIAN_POINT('Ctrl Pts',(-43.0145657452096,54.3116908534688,-448.044287311638));
#35486=CARTESIAN_POINT('Ctrl Pts',(-43.033961062082,54.3335117194169,-448.011782797623));
#35487=CARTESIAN_POINT('Ctrl Pts',(-43.0533558928743,54.3553329875833,-447.979278207444));
#35488=CARTESIAN_POINT('Ctrl Pts',(-43.725941731794,55.1120643101229,-446.852064091059));
#35489=CARTESIAN_POINT('Ctrl Pts',(-44.3979432331023,55.8692792318855,-445.724758430936));
#35490=CARTESIAN_POINT('Ctrl Pts',(-45.0698032706076,56.6264489656385,-444.597331241255));
#35491=CARTESIAN_POINT('Ctrl Pts',(-45.0731946234504,56.6302709368613,-444.591640318754));
#35492=CARTESIAN_POINT('Ctrl Pts',(-45.076585972684,56.6340929069347,-444.585949393156));
#35493=CARTESIAN_POINT('Ctrl Pts',(-45.0799773183656,56.6379148757911,-444.580258464457));
#35494=CARTESIAN_POINT('Ctrl Pts',(-45.0804692403649,56.63846926061,-444.579432982985));
#35495=CARTESIAN_POINT('Ctrl Pts',(-45.0809611622896,56.6390236454031,-444.578607501448));
#35496=CARTESIAN_POINT('Ctrl Pts',(-45.0816336415163,56.6397815142388,-444.577479031083));
#35497=CARTESIAN_POINT('Ctrl Pts',(-45.0818141988828,56.6399849983033,-444.577176042312));
#35498=CARTESIAN_POINT('Ctrl Pts',(-45.7904609111333,57.43861383136,-443.388013734489));
#35499=CARTESIAN_POINT('Ctrl Pts',(-46.498772170558,58.2369857607961,-442.199018996768));
#35500=CARTESIAN_POINT('Ctrl Pts',(-47.2095301480132,59.0375097782374,-441.006896364563));
#35501=CARTESIAN_POINT('Ctrl Pts',(-47.2114706948088,59.0396954042171,-441.003641579351));
#35502=CARTESIAN_POINT('Ctrl Pts',(-47.2561793755078,59.0900504130787,-440.928654042424));
#35503=CARTESIAN_POINT('Ctrl Pts',(-47.2989475056031,59.1382197962114,-440.856921289753));
#35504=CARTESIAN_POINT('Ctrl Pts',(-47.3417156356984,59.1863891793441,-440.785188537082));
#35505=CARTESIAN_POINT('Ctrl Pts',(-33.882499227078,44.8150532196688,-462.499999999992));
#35506=CARTESIAN_POINT('Ctrl Pts',(-34.5897963205529,45.6187146263589,-461.305295910369));
#35507=CARTESIAN_POINT('Ctrl Pts',(-35.2995473263181,46.4208713719593,-460.11091477585));
#35508=CARTESIAN_POINT('Ctrl Pts',(-36.004497088199,47.2265044265567,-458.915337870982));
#35509=CARTESIAN_POINT('Ctrl Pts',(-36.0341630913862,47.2604074279587,-458.865025082485));
#35510=CARTESIAN_POINT('Ctrl Pts',(-36.06382059298,47.2943165848991,-458.814710176593));
#35511=CARTESIAN_POINT('Ctrl Pts',(-36.0934695146101,47.3282319170015,-458.764393149568));
#35512=CARTESIAN_POINT('Ctrl Pts',(-36.4346832245758,47.7185454817157,-458.185321179272));
#35513=CARTESIAN_POINT('Ctrl Pts',(-36.7747601945371,48.109677063011,-457.605968201868));
#35514=CARTESIAN_POINT('Ctrl Pts',(-37.1135830980392,48.5016557071232,-457.026328952538));
#35515=CARTESIAN_POINT('Ctrl Pts',(-37.2809252930373,48.6952511400767,-456.740049296448));
#35516=CARTESIAN_POINT('Ctrl Pts',(-37.4479616662434,48.8890531643603,-456.453699826454));
#35517=CARTESIAN_POINT('Ctrl Pts',(-37.6146781577475,49.0830652430437,-456.167279920779));
#35518=CARTESIAN_POINT('Ctrl Pts',(-37.7773711153053,49.2723950363843,-455.887772469913));
#35519=CARTESIAN_POINT('Ctrl Pts',(-37.9397594650648,49.4619248602184,-455.608197945846));
#35520=CARTESIAN_POINT('Ctrl Pts',(-38.1018297888824,49.6516580582508,-455.328555701444));
#35521=CARTESIAN_POINT('Ctrl Pts',(-38.3105323208151,49.8959828543535,-454.968452487807));
#35522=CARTESIAN_POINT('Ctrl Pts',(-38.5187074679136,50.140644897714,-454.608236973389));
#35523=CARTESIAN_POINT('Ctrl Pts',(-38.7265655086456,50.3854835677273,-454.247953136177));
#35524=CARTESIAN_POINT('Ctrl Pts',(-39.2089318788736,50.9536691434688,-453.411859395487));
#35525=CARTESIAN_POINT('Ctrl Pts',(-39.6895895863211,51.5228061244817,-452.575397552201));
#35526=CARTESIAN_POINT('Ctrl Pts',(-40.1711841106882,52.0908820466578,-451.739120208895));
#35527=CARTESIAN_POINT('Ctrl Pts',(-40.4609157135043,52.4326416371961,-451.23600822814));
#35528=CARTESIAN_POINT('Ctrl Pts',(-40.7508626122354,52.7742567903562,-450.732936537627));
#35529=CARTESIAN_POINT('Ctrl Pts',(-41.0408883415266,53.1158294556676,-450.229873897835));
#35530=CARTESIAN_POINT('Ctrl Pts',(-41.4389491499721,53.5846385217771,-449.539419566132));
#35531=CARTESIAN_POINT('Ctrl Pts',(-41.8371805402333,54.0533595457502,-448.848986303267));
#35532=CARTESIAN_POINT('Ctrl Pts',(-42.2352610710188,54.5222446334621,-448.158498944552));
#35533=CARTESIAN_POINT('Ctrl Pts',(-42.23564501511,54.5226968677337,-448.15783297744));
#35534=CARTESIAN_POINT('Ctrl Pts',(-42.2360289590583,54.5231491021588,-448.157167010277));
#35535=CARTESIAN_POINT('Ctrl Pts',(-42.236412902864,54.5236013367372,-448.156501043064));
#35536=CARTESIAN_POINT('Ctrl Pts',(-42.251480944002,54.541349478861,-448.130364871002));
#35537=CARTESIAN_POINT('Ctrl Pts',(-42.2665487655235,54.5590978571757,-448.104228620798));
#35538=CARTESIAN_POINT('Ctrl Pts',(-42.2816163693486,54.5768464677822,-448.078092291274));
#35539=CARTESIAN_POINT('Ctrl Pts',(-42.3003552207916,54.5989195579256,-448.045587800056));
#35540=CARTESIAN_POINT('Ctrl Pts',(-42.3190937355299,54.6209930073476,-448.013083186158));
#35541=CARTESIAN_POINT('Ctrl Pts',(-42.3378319172539,54.6430668085493,-447.980578447317));
#35542=CARTESIAN_POINT('Ctrl Pts',(-42.9876460769867,55.40855562659,-446.853359175542));
#35543=CARTESIAN_POINT('Ctrl Pts',(-43.6370600294435,56.1744673877555,-445.72598971932));
#35544=CARTESIAN_POINT('Ctrl Pts',(-44.2862257462271,56.9404901210901,-444.598375225355));
#35545=CARTESIAN_POINT('Ctrl Pts',(-44.2895025447805,56.9443567796637,-444.592683357397));
#35546=CARTESIAN_POINT('Ctrl Pts',(-44.2927793370035,56.9482234410669,-444.586991483194));
#35547=CARTESIAN_POINT('Ctrl Pts',(-44.2960561229152,56.9520901052595,-444.581299602734));
#35548=CARTESIAN_POINT('Ctrl Pts',(-44.2965314277732,56.9526509732333,-444.580473983208));
#35549=CARTESIAN_POINT('Ctrl Pts',(-44.2970067324983,56.9532118412657,-444.579648363549));
#35550=CARTESIAN_POINT('Ctrl Pts',(-44.2976564951886,56.9539785730952,-444.578519704276));
#35551=CARTESIAN_POINT('Ctrl Pts',(-44.2978309532686,56.9541844368416,-444.578216664775));
#35552=CARTESIAN_POINT('Ctrl Pts',(-44.9825393171837,57.7621530264513,-443.388855217941));
#35553=CARTESIAN_POINT('Ctrl Pts',(-45.6667975667759,58.5700373708246,-442.199523556902));
#35554=CARTESIAN_POINT('Ctrl Pts',(-46.3537037290544,59.3801133786364,-441.006942922665));
#35555=CARTESIAN_POINT('Ctrl Pts',(-46.3555791565611,59.3823250839859,-441.003686886098));
#35556=CARTESIAN_POINT('Ctrl Pts',(-46.3987875888851,59.4332809422084,-440.928670498321));
#35557=CARTESIAN_POINT('Ctrl Pts',(-46.4401205878902,59.4820250952344,-440.856910147053));
#35558=CARTESIAN_POINT('Ctrl Pts',(-46.4814535868953,59.5307692482604,-440.785149795784));
#35559=CARTESIAN_POINT('Ctrl Pts',(-33.4710017122312,44.9624982997247,-462.499999999992));
#35560=CARTESIAN_POINT('Ctrl Pts',(-34.1498065842261,45.7760949547167,-461.305574764512));
#35561=CARTESIAN_POINT('Ctrl Pts',(-34.8302145362503,46.5890736375712,-460.111073961072));
#35562=CARTESIAN_POINT('Ctrl Pts',(-35.5071397368667,47.4047760112341,-458.915497269838));
#35563=CARTESIAN_POINT('Ctrl Pts',(-35.5356263982502,47.4391027541106,-458.865184490332));
#35564=CARTESIAN_POINT('Ctrl Pts',(-35.5641068927283,47.4734343199053,-458.814869805673));
#35565=CARTESIAN_POINT('Ctrl Pts',(-35.5925811583742,47.5077707165236,-458.764553216379));
#35566=CARTESIAN_POINT('Ctrl Pts',(-35.9202763757838,47.9029300893719,-458.185486283692));
#35567=CARTESIAN_POINT('Ctrl Pts',(-36.2471461026656,48.2987294808301,-457.606166988185));
#35568=CARTESIAN_POINT('Ctrl Pts',(-36.5730989065517,48.6951797757475,-457.026596718414));
#35569=CARTESIAN_POINT('Ctrl Pts',(-36.7340846519198,48.8909837248705,-456.740351130832));
#35570=CARTESIAN_POINT('Ctrl Pts',(-36.8948468485331,49.0869464039666,-456.454044346223));
#35571=CARTESIAN_POINT('Ctrl Pts',(-37.0553745659741,49.2830690882183,-456.167676545631));
#35572=CARTESIAN_POINT('Ctrl Pts',(-37.2120281092728,49.4744585497958,-455.888219942345));
#35573=CARTESIAN_POINT('Ctrl Pts',(-37.3684583839647,49.6660003759221,-455.608705238052));
#35574=CARTESIAN_POINT('Ctrl Pts',(-37.5246547051888,49.857695944655,-455.329132497536));
#35575=CARTESIAN_POINT('Ctrl Pts',(-37.7257931181328,50.1045477409151,-454.969118786015));
#35576=CARTESIAN_POINT('Ctrl Pts',(-37.9265435396957,50.3516544917298,-454.609008828603));
#35577=CARTESIAN_POINT('Ctrl Pts',(-38.1270461953369,50.5989043899216,-454.248833716317));
#35578=CARTESIAN_POINT('Ctrl Pts',(-38.5923432696388,51.1726855893882,-453.412992288444));
#35579=CARTESIAN_POINT('Ctrl Pts',(-39.0563044147987,51.7472381853159,-452.57679969215));
#35580=CARTESIAN_POINT('Ctrl Pts',(-39.5207100112726,52.3211556802638,-451.740649315997));
#35581=CARTESIAN_POINT('Ctrl Pts',(-39.8001006002745,52.6664296135875,-451.237613719826));
#35582=CARTESIAN_POINT('Ctrl Pts',(-40.0796597373392,53.0115890944338,-450.734595265531));
#35583=CARTESIAN_POINT('Ctrl Pts',(-40.3592902725819,53.356713226554,-450.231566929635));
#35584=CARTESIAN_POINT('Ctrl Pts',(-40.7430836594543,53.8303966869201,-449.541159680087));
#35585=CARTESIAN_POINT('Ctrl Pts',(-41.1270436081776,54.3040019309654,-448.85073965213));
#35586=CARTESIAN_POINT('Ctrl Pts',(-41.5109640329818,54.7777171498825,-448.16024502308));
#35587=CARTESIAN_POINT('Ctrl Pts',(-41.5113343198136,54.7781740427599,-448.159579048956));
#35588=CARTESIAN_POINT('Ctrl Pts',(-41.5117046066051,54.7786309357411,-448.158913074762));
#35589=CARTESIAN_POINT('Ctrl Pts',(-41.5120748933564,54.7790878288258,-448.158247100498));
#35590=CARTESIAN_POINT('Ctrl Pts',(-41.5266069574702,54.7970187960456,-448.132110651728));
#35591=CARTESIAN_POINT('Ctrl Pts',(-41.5411389597152,54.8149499226548,-448.10597409512));
#35592=CARTESIAN_POINT('Ctrl Pts',(-41.5556708969731,54.8328812087858,-448.079837428255));
#35593=CARTESIAN_POINT('Ctrl Pts',(-41.5737435657675,54.8551814836599,-448.0473325175));
#35594=CARTESIAN_POINT('Ctrl Pts',(-41.5918161340486,54.8774820052618,-448.014827436212));
#35595=CARTESIAN_POINT('Ctrl Pts',(-41.609888595815,54.8997827738486,-447.982322179732));
#35596=CARTESIAN_POINT('Ctrl Pts',(-42.2366165105127,55.6731425060908,-446.85508495696));
#35597=CARTESIAN_POINT('Ctrl Pts',(-42.8632166744256,56.446799156781,-445.727637147225));
#35598=CARTESIAN_POINT('Ctrl Pts',(-43.4894364238166,57.2207642094785,-444.599783822231));
#35599=CARTESIAN_POINT('Ctrl Pts',(-43.492597397842,57.2246709585559,-444.594090748724));
#35600=CARTESIAN_POINT('Ctrl Pts',(-43.4957583621677,57.228577715493,-444.588397664883));
#35601=CARTESIAN_POINT('Ctrl Pts',(-43.4989193167611,57.2324844802916,-444.582704570682));
#35602=CARTESIAN_POINT('Ctrl Pts',(-43.4993778200367,57.2330511649446,-444.5818787751));
#35603=CARTESIAN_POINT('Ctrl Pts',(-43.4998363231075,57.233617849763,-444.581052979299));
#35604=CARTESIAN_POINT('Ctrl Pts',(-43.5004631170844,57.2343925335459,-444.579924079114));
#35605=CARTESIAN_POINT('Ctrl Pts',(-43.5006314081677,57.2346005323672,-444.579620974917));
#35606=CARTESIAN_POINT('Ctrl Pts',(-44.1611356691744,58.0509488636593,-443.390005567788));
#35607=CARTESIAN_POINT('Ctrl Pts',(-44.821046186353,58.8674324443465,-442.200240815627));
#35608=CARTESIAN_POINT('Ctrl Pts',(-45.4838216333574,59.686214391916,-441.007046063224));
#35609=CARTESIAN_POINT('Ctrl Pts',(-45.4856311802341,59.6884498672306,-441.00378834862));
#35610=CARTESIAN_POINT('Ctrl Pts',(-45.5273218264009,59.7399533800503,-440.928733269294));
#35611=CARTESIAN_POINT('Ctrl Pts',(-45.5672029177492,59.7892214170893,-440.856935905857));
#35612=CARTESIAN_POINT('Ctrl Pts',(-45.6070840090976,59.8384894541283,-440.78513854242));
#35613=CARTESIAN_POINT('Ctrl Pts',(-33.0533836161765,45.091854154172,-462.499999999992));
#35614=CARTESIAN_POINT('Ctrl Pts',(-33.7034151132609,45.9143089978342,-461.305736187933));
#35615=CARTESIAN_POINT('Ctrl Pts',(-34.3544003661019,46.7366884856134,-460.111197234966));
#35616=CARTESIAN_POINT('Ctrl Pts',(-35.0030466122211,47.5611021033272,-458.915728574456));
#35617=CARTESIAN_POINT('Ctrl Pts',(-35.0303432263138,47.5957954365733,-458.865420341145));
#35618=CARTESIAN_POINT('Ctrl Pts',(-35.0576356987778,47.6304923717441,-458.81511046151));
#35619=CARTESIAN_POINT('Ctrl Pts',(-35.0849239853749,47.6651929130949,-458.764798934386));
#35620=CARTESIAN_POINT('Ctrl Pts',(-35.3989703990889,48.0645430344869,-458.185790259525));
#35621=CARTESIAN_POINT('Ctrl Pts',(-35.7124617861774,48.464371018814,-457.606563255973));
#35622=CARTESIAN_POINT('Ctrl Pts',(-36.0253343395421,48.8646819472439,-457.027116886978));
#35623=CARTESIAN_POINT('Ctrl Pts',(-36.1798598432595,49.0623926354905,-456.740932493099));
#35624=CARTESIAN_POINT('Ctrl Pts',(-36.3342345379915,49.26022107364,-456.454694617896));
#35625=CARTESIAN_POINT('Ctrl Pts',(-36.4884508294031,49.4581678377631,-456.168403151226));
#35626=CARTESIAN_POINT('Ctrl Pts',(-36.638945266558,49.6513373568889,-455.88902103962));
#35627=CARTESIAN_POINT('Ctrl Pts',(-36.7892888905276,49.8446195462205,-455.609587898822));
#35628=CARTESIAN_POINT('Ctrl Pts',(-36.9394739770257,50.0380151880987,-455.330103495726));
#35629=CARTESIAN_POINT('Ctrl Pts',(-37.1328715532901,50.2870562165485,-454.970203538794));
#35630=CARTESIAN_POINT('Ctrl Pts',(-37.3260061809514,50.5362853956562,-454.610218565813));
#35631=CARTESIAN_POINT('Ctrl Pts',(-37.5189638217216,50.785631966803,-454.250167529876));
#35632=CARTESIAN_POINT('Ctrl Pts',(-37.9667515351936,51.3642788164959,-453.414614040146));
#35633=CARTESIAN_POINT('Ctrl Pts',(-38.4135839406132,51.943558591785,-452.57870439064));
#35634=CARTESIAN_POINT('Ctrl Pts',(-38.8605715509455,52.5225745434955,-451.742681745474));
#35635=CARTESIAN_POINT('Ctrl Pts',(-39.1294833226286,52.8709157543212,-451.239722993414));
#35636=CARTESIAN_POINT('Ctrl Pts',(-39.3985305366766,53.2191901195012,-450.736738959138));
#35637=CARTESIAN_POINT('Ctrl Pts',(-39.6676464559522,53.5674526320097,-450.233712353502));
#35638=CARTESIAN_POINT('Ctrl Pts',(-40.0370085144638,54.0454435248148,-449.54330747874));
#35639=CARTESIAN_POINT('Ctrl Pts',(-40.4065400300739,54.5233975701954,-448.852829696241));
#35640=CARTESIAN_POINT('Ctrl Pts',(-40.7761244907476,55.0014367516422,-448.162244300311));
#35641=CARTESIAN_POINT('Ctrl Pts',(-40.7764809507071,55.0018978149318,-448.161578238643));
#35642=CARTESIAN_POINT('Ctrl Pts',(-40.7768374107112,55.0023588783023,-448.160912176875));
#35643=CARTESIAN_POINT('Ctrl Pts',(-40.7771938707602,55.0028199417536,-448.160246115005));
#35644=CARTESIAN_POINT('Ctrl Pts',(-40.7911832999486,55.020914576818,-448.134106228125));
#35645=CARTESIAN_POINT('Ctrl Pts',(-40.8051727983377,55.0390093362169,-448.10796618588));
#35646=CARTESIAN_POINT('Ctrl Pts',(-40.8191623586508,55.057104222479,-448.081825985748));
#35647=CARTESIAN_POINT('Ctrl Pts',(-40.8365604994238,55.0796079589375,-448.049316680841));
#35648=CARTESIAN_POINT('Ctrl Pts',(-40.8539587359728,55.1021118916113,-448.016807131734));
#35649=CARTESIAN_POINT('Ctrl Pts',(-40.8713570542966,55.1246160253655,-447.984297333575));
#35650=CARTESIAN_POINT('Ctrl Pts',(-41.4747066091777,55.9050281796226,-446.856902611653));
#35651=CARTESIAN_POINT('Ctrl Pts',(-42.0781549044513,56.6856820489916,-445.729208498906));
#35652=CARTESIAN_POINT('Ctrl Pts',(-42.681115280234,57.4667812939235,-444.601011806645));
#35653=CARTESIAN_POINT('Ctrl Pts',(-42.6841588477485,57.4707240543153,-444.59531699992));
#35654=CARTESIAN_POINT('Ctrl Pts',(-42.6872024028231,57.4746668260569,-444.589622180388));
#35655=CARTESIAN_POINT('Ctrl Pts',(-42.6902459453823,57.4786096091744,-444.583927348021));
#35656=CARTESIAN_POINT('Ctrl Pts',(-42.6906874177893,57.4791815183622,-444.583101300314));
#35657=CARTESIAN_POINT('Ctrl Pts',(-42.6911288899329,57.4797534277893,-444.582275252337));
#35658=CARTESIAN_POINT('Ctrl Pts',(-42.6917324017885,57.4805352539479,-444.581146007343));
#35659=CARTESIAN_POINT('Ctrl Pts',(-42.6918944417284,57.480745170472,-444.580842810561));
#35660=CARTESIAN_POINT('Ctrl Pts',(-43.3278643503816,58.3046200899417,-443.390863995632));
#35661=CARTESIAN_POINT('Ctrl Pts',(-43.9631249009979,59.1287818793436,-442.200627878454));
#35662=CARTESIAN_POINT('Ctrl Pts',(-44.6013941965172,59.9552283282957,-441.006936223393));
#35663=CARTESIAN_POINT('Ctrl Pts',(-44.6031368371902,59.957484729313,-441.003677151942));
#35664=CARTESIAN_POINT('Ctrl Pts',(-44.6432860563195,60.0094703469446,-440.928590807858));
#35665=CARTESIAN_POINT('Ctrl Pts',(-44.6816926252475,60.0591995633562,-440.85676353669));
#35666=CARTESIAN_POINT('Ctrl Pts',(-44.7200991941757,60.1089287797678,-440.784936265522));
#35667=CARTESIAN_POINT('Ctrl Pts',(-33.0529806979711,45.0919789381448,-462.499999999992));
#35668=CARTESIAN_POINT('Ctrl Pts',(-33.7029844346161,45.9144423270676,-461.305736343562));
#35669=CARTESIAN_POINT('Ctrl Pts',(-34.3539413007462,46.7368308832956,-460.111197353865));
#35670=CARTESIAN_POINT('Ctrl Pts',(-35.0025602634613,47.5612529042377,-458.915728797683));
#35671=CARTESIAN_POINT('Ctrl Pts',(-35.029855729402,47.5959465911122,-458.865420568762));
#35672=CARTESIAN_POINT('Ctrl Pts',(-35.0571470556675,47.6306438787335,-458.815110693767));
#35673=CARTESIAN_POINT('Ctrl Pts',(-35.0844341980371,47.6653447713533,-458.764799171531));
#35674=CARTESIAN_POINT('Ctrl Pts',(-35.3984674434415,48.0646989353141,-458.185790552926));
#35675=CARTESIAN_POINT('Ctrl Pts',(-35.7119459231226,48.4645308057789,-457.606563638471));
#35676=CARTESIAN_POINT('Ctrl Pts',(-36.0248058566361,48.864845458328,-457.027117389066));
#35677=CARTESIAN_POINT('Ctrl Pts',(-36.1793251274998,49.0625579858903,-456.740933054251));
#35678=CARTESIAN_POINT('Ctrl Pts',(-36.3336936595474,49.2603882238248,-456.454695245554));
#35679=CARTESIAN_POINT('Ctrl Pts',(-36.4879038616631,49.4583367475293,-456.168403852554));
#35680=CARTESIAN_POINT('Ctrl Pts',(-36.638392356481,49.6515079837707,-455.889021812838));
#35681=CARTESIAN_POINT('Ctrl Pts',(-36.7887301080094,49.8447918519287,-455.609588750752));
#35682=CARTESIAN_POINT('Ctrl Pts',(-36.9389093948188,50.0381891337709,-455.3301044329));
#35683=CARTESIAN_POINT('Ctrl Pts',(-37.1322995026599,50.2872322740483,-454.970204585739));
#35684=CARTESIAN_POINT('Ctrl Pts',(-37.3254267825243,50.5364635005466,-454.61021973336));
#35685=CARTESIAN_POINT('Ctrl Pts',(-37.5183771437858,50.7858120942428,-454.250168817144));
#35686=CARTESIAN_POINT('Ctrl Pts',(-37.966147964044,51.364463637571,-453.414615605247));
#35687=CARTESIAN_POINT('Ctrl Pts',(-38.4129638434758,51.9437479729391,-452.578706228737));
#35688=CARTESIAN_POINT('Ctrl Pts',(-38.8599346489484,52.5227688428812,-451.742683706805));
#35689=CARTESIAN_POINT('Ctrl Pts',(-39.1288363106765,52.8711130125594,-451.239725028884));
#35690=CARTESIAN_POINT('Ctrl Pts',(-39.3978733828416,53.2193903825393,-450.736741027798));
#35691=CARTESIAN_POINT('Ctrl Pts',(-39.66697915764,53.5676559225319,-450.233714423801));
#35692=CARTESIAN_POINT('Ctrl Pts',(-40.0363272928394,54.0456509705641,-449.543309551288));
#35693=CARTESIAN_POINT('Ctrl Pts',(-40.4058448879359,54.5236092111141,-448.852831713002));
#35694=CARTESIAN_POINT('Ctrl Pts',(-40.7754155172909,55.0016525637938,-448.162246229423));
#35695=CARTESIAN_POINT('Ctrl Pts',(-40.7757719639103,55.0021136311065,-448.161580167671));
#35696=CARTESIAN_POINT('Ctrl Pts',(-40.7761284105743,55.0025746985001,-448.160914105818));
#35697=CARTESIAN_POINT('Ctrl Pts',(-40.7764848572834,55.0030357659744,-448.160248043864));
#35698=CARTESIAN_POINT('Ctrl Pts',(-40.7904737629383,55.0211305589256,-448.134108153664));
#35699=CARTESIAN_POINT('Ctrl Pts',(-40.8044627379204,55.0392254761776,-448.107968108053));
#35700=CARTESIAN_POINT('Ctrl Pts',(-40.8184517749489,55.0573205202613,-448.081827904509));
#35701=CARTESIAN_POINT('Ctrl Pts',(-40.8358492649381,55.0798244529948,-448.049318595359));
#35702=CARTESIAN_POINT('Ctrl Pts',(-40.8532468508926,55.102328581895,-448.016809041938));
#35703=CARTESIAN_POINT('Ctrl Pts',(-40.8706445188036,55.1248329118314,-447.984299239393));
#35704=CARTESIAN_POINT('Ctrl Pts',(-41.4739715182697,55.9052518694137,-446.856904365388));
#35705=CARTESIAN_POINT('Ctrl Pts',(-42.0773974766002,56.6859124889152,-445.729210014854));
#35706=CARTESIAN_POINT('Ctrl Pts',(-42.6803354117444,57.4670186160727,-444.601012991219));
#35707=CARTESIAN_POINT('Ctrl Pts',(-42.6833788659852,57.4709614112041,-444.595318182822));
#35708=CARTESIAN_POINT('Ctrl Pts',(-42.6864223077834,57.4749042176885,-444.589623361614));
#35709=CARTESIAN_POINT('Ctrl Pts',(-42.6894657370635,57.4788470355523,-444.58392852757));
#35710=CARTESIAN_POINT('Ctrl Pts',(-42.6899071930391,57.4794189497801,-444.58310247962));
#35711=CARTESIAN_POINT('Ctrl Pts',(-42.6903486487513,57.4799908642473,-444.582276431399));
#35712=CARTESIAN_POINT('Ctrl Pts',(-42.6909521381443,57.4807726972959,-444.581147186073));
#35713=CARTESIAN_POINT('Ctrl Pts',(-42.6911141720531,57.48098261567,-444.5808439892));
#35714=CARTESIAN_POINT('Ctrl Pts',(-43.3270604099691,58.304864795902,-443.390864823559));
#35715=CARTESIAN_POINT('Ctrl Pts',(-43.9622971783327,59.1290339922837,-442.200628251578));
#35716=CARTESIAN_POINT('Ctrl Pts',(-44.6005428302862,59.9554878348756,-441.006936117221));
#35717=CARTESIAN_POINT('Ctrl Pts',(-44.602285406408,59.957744256079,-441.003677044461));
#35718=CARTESIAN_POINT('Ctrl Pts',(-44.6424331383656,60.0097303387795,-440.92859067022));
#35719=CARTESIAN_POINT('Ctrl Pts',(-44.6808382846717,60.059460000074,-440.856763370203));
#35720=CARTESIAN_POINT('Ctrl Pts',(-44.7192434309778,60.1091896613684,-440.784936070187));
#35721=CARTESIAN_POINT('Ctrl Pts',(-32.6383541991618,45.2203697961812,-462.499999999991));
#35722=CARTESIAN_POINT('Ctrl Pts',(-33.2597909482979,46.0516256021186,-461.305896380459));
#35723=CARTESIAN_POINT('Ctrl Pts',(-33.8815365596243,46.8833446286893,-460.11131967209));
#35724=CARTESIAN_POINT('Ctrl Pts',(-34.5020794511689,47.7164126393723,-458.915958576709));
#35725=CARTESIAN_POINT('Ctrl Pts',(-34.5281934076432,47.751470170556,-458.865654870001));
#35726=CARTESIAN_POINT('Ctrl Pts',(-34.55430523456,47.7865300904887,-458.815349774274));
#35727=CARTESIAN_POINT('Ctrl Pts',(-34.5804149052619,47.8215923998134,-458.76504328668));
#35728=CARTESIAN_POINT('Ctrl Pts',(-34.8808972539054,48.2251059168955,-458.18609260911));
#35729=CARTESIAN_POINT('Ctrl Pts',(-35.1810932773081,48.6289361814173,-457.606957435406));
#35730=CARTESIAN_POINT('Ctrl Pts',(-35.4809666250378,49.0330825307212,-457.02763430117));
#35731=CARTESIAN_POINT('Ctrl Pts',(-35.6290719145911,49.2326875057504,-456.741510772053));
#35732=CARTESIAN_POINT('Ctrl Pts',(-35.7770986636649,49.4323695190089,-456.455341427537));
#35733=CARTESIAN_POINT('Ctrl Pts',(-35.9250425936302,49.6321284546669,-456.169125866008));
#35734=CARTESIAN_POINT('Ctrl Pts',(-36.0694160464399,49.8270664103998,-455.889817827648));
#35735=CARTESIAN_POINT('Ctrl Pts',(-36.2137106732404,50.0220776044787,-455.610465784224));
#35736=CARTESIAN_POINT('Ctrl Pts',(-36.3579216923215,50.2171622298651,-455.331069204655));
#35737=CARTESIAN_POINT('Ctrl Pts',(-36.5436262932987,50.4683782100658,-454.971282340559));
#35738=CARTESIAN_POINT('Ctrl Pts',(-36.7291921822414,50.7197159827528,-454.61142161106));
#35739=CARTESIAN_POINT('Ctrl Pts',(-36.9146514253514,50.9711455673303,-454.251493908347));
#35740=CARTESIAN_POINT('Ctrl Pts',(-37.3450379603595,51.5546263682339,-453.416226632226));
#35741=CARTESIAN_POINT('Ctrl Pts',(-37.7748474534568,52.1386025657758,-452.580598193939));
#35742=CARTESIAN_POINT('Ctrl Pts',(-38.2045250964898,52.7226837998791,-451.744702485881));
#35743=CARTESIAN_POINT('Ctrl Pts',(-38.4630230359624,53.0740723302074,-451.241820100329));
#35744=CARTESIAN_POINT('Ctrl Pts',(-38.7216235428773,53.4254413601958,-450.738870235561));
#35745=CARTESIAN_POINT('Ctrl Pts',(-38.980290086803,53.7768219194506,-450.235845286766));
#35746=CARTESIAN_POINT('Ctrl Pts',(-39.3353103598129,54.2590923367369,-449.545442686022));
#35747=CARTESIAN_POINT('Ctrl Pts',(-39.6905029782764,54.7413670799393,-448.85490737208));
#35748=CARTESIAN_POINT('Ctrl Pts',(-40.0458403977317,55.2237023319474,-448.164231613875));
#35749=CARTESIAN_POINT('Ctrl Pts',(-40.0461831165839,55.2241675387477,-448.163565465054));
#35750=CARTESIAN_POINT('Ctrl Pts',(-40.0465258355652,55.2246327456062,-448.162899316101));
#35751=CARTESIAN_POINT('Ctrl Pts',(-40.0468685546759,55.2250979525229,-448.162233167017));
#35752=CARTESIAN_POINT('Ctrl Pts',(-40.0603187147842,55.2433551996868,-448.136089857356));
#35753=CARTESIAN_POINT('Ctrl Pts',(-40.0737690742939,55.2616125364301,-448.109946345064));
#35754=CARTESIAN_POINT('Ctrl Pts',(-40.0872196217972,55.2798699676587,-448.08380262752));
#35755=CARTESIAN_POINT('Ctrl Pts',(-40.1039474183612,55.3025758534449,-448.051288948177));
#35756=CARTESIAN_POINT('Ctrl Pts',(-40.1206755056895,55.3252818853689,-448.018774951378));
#35757=CARTESIAN_POINT('Ctrl Pts',(-40.1374038618344,55.347988072869,-447.98626063208));
#35758=CARTESIAN_POINT('Ctrl Pts',(-40.7175200573205,56.135407170867,-446.858709123344));
#35759=CARTESIAN_POINT('Ctrl Pts',(-41.2979599832958,56.9230132620828,-445.730769918261));
#35760=CARTESIAN_POINT('Ctrl Pts',(-41.8778052042609,57.7112007315841,-444.602231795743));
#35761=CARTESIAN_POINT('Ctrl Pts',(-41.8807320932388,57.715179271259,-444.596535265579));
#35762=CARTESIAN_POINT('Ctrl Pts',(-41.883658967055,57.719157825749,-444.590838720151));
#35763=CARTESIAN_POINT('Ctrl Pts',(-41.8865858255911,57.7231363951044,-444.585142159434));
#35764=CARTESIAN_POINT('Ctrl Pts',(-41.8870103727291,57.7237134951632,-444.584315861025));
#35765=CARTESIAN_POINT('Ctrl Pts',(-41.8874349195456,57.7242905955347,-444.583489562295));
#35766=CARTESIAN_POINT('Ctrl Pts',(-41.8880152936402,57.7250795180474,-444.582359974441));
#35767=CARTESIAN_POINT('Ctrl Pts',(-41.8881711211969,57.7252913399177,-444.582056685595));
#35768=CARTESIAN_POINT('Ctrl Pts',(-42.4997588024213,58.5566443504447,-443.391716515218));
#35769=CARTESIAN_POINT('Ctrl Pts',(-43.110522288096,59.3884347749287,-442.201011894464));
#35770=CARTESIAN_POINT('Ctrl Pts',(-43.7244373063526,60.2224959997518,-441.006826656209));
#35771=CARTESIAN_POINT('Ctrl Pts',(-43.726113455465,60.2247731907088,-441.003566236976));
#35772=CARTESIAN_POINT('Ctrl Pts',(-43.7647308003352,60.2772377852853,-440.928448837104));
#35773=CARTESIAN_POINT('Ctrl Pts',(-43.8016719849895,60.3274251889655,-440.856591858102));
#35774=CARTESIAN_POINT('Ctrl Pts',(-43.8386131696438,60.3776125926457,-440.784734879101));
#35775=CARTESIAN_POINT('Ctrl Pts',(-32.2184964333868,45.3306825375905,-462.499999999992));
#35776=CARTESIAN_POINT('Ctrl Pts',(-32.8111445755329,46.1696524166233,-461.305940121841));
#35777=CARTESIAN_POINT('Ctrl Pts',(-33.4036575962112,47.0092828772597,-460.111406153985));
#35778=CARTESIAN_POINT('Ctrl Pts',(-33.9959283196953,47.8496414198625,-458.916258639274));
#35779=CARTESIAN_POINT('Ctrl Pts',(-34.0208525144688,47.8850057543887,-458.86596392056));
#35780=CARTESIAN_POINT('Ctrl Pts',(-34.0457762803665,47.9203713782159,-458.815668115338));
#35781=CARTESIAN_POINT('Ctrl Pts',(-34.0706996094887,47.9557382963416,-458.76537121323));
#35782=CARTESIAN_POINT('Ctrl Pts',(-34.3575289822595,48.3627573945163,-458.18653084992));
#35783=CARTESIAN_POINT('Ctrl Pts',(-34.644299674474,48.7699482318228,-457.607545041494));
#35784=CARTESIAN_POINT('Ctrl Pts',(-34.9310044180742,49.1773166053379,-457.028398945302));
#35785=CARTESIAN_POINT('Ctrl Pts',(-35.0726058287653,49.3785129149502,-456.742362854001));
#35786=CARTESIAN_POINT('Ctrl Pts',(-35.214191342309,49.5797524594164,-456.456287701493));
#35787=CARTESIAN_POINT('Ctrl Pts',(-35.355760189644,49.7810359012113,-456.170171716108));
#35788=CARTESIAN_POINT('Ctrl Pts',(-35.4939124159966,49.9774615706671,-455.890960850722));
#35789=CARTESIAN_POINT('Ctrl Pts',(-35.632048820103,50.1739290262489,-455.611711108655));
#35790=CARTESIAN_POINT('Ctrl Pts',(-35.7701677782543,50.3704392242245,-455.332420665377));
#35791=CARTESIAN_POINT('Ctrl Pts',(-35.9480274603671,50.6234909544982,-454.97277047598));
#35792=CARTESIAN_POINT('Ctrl Pts',(-36.1258581314242,50.8766135926294,-454.613052778229));
#35793=CARTESIAN_POINT('Ctrl Pts',(-36.3036537099415,51.1298101455982,-454.253263180005));
#35794=CARTESIAN_POINT('Ctrl Pts',(-36.7162555392955,51.717391466868,-453.418316396471));
#35795=CARTESIAN_POINT('Ctrl Pts',(-37.1286652611844,52.3053719738747,-452.58298184057));
#35796=CARTESIAN_POINT('Ctrl Pts',(-37.54085746243,52.8937711567081,-451.747213467217));
#35797=CARTESIAN_POINT('Ctrl Pts',(-37.7888360026596,53.2477574038771,-451.244407687371));
#35798=CARTESIAN_POINT('Ctrl Pts',(-38.0368974401792,53.6017882593027,-450.741473324899));
#35799=CARTESIAN_POINT('Ctrl Pts',(-38.2850266726511,53.9558697509131,-450.238417879064));
#35800=CARTESIAN_POINT('Ctrl Pts',(-38.6255844677064,54.441847202467,-449.547973421078));
#35801=CARTESIAN_POINT('Ctrl Pts',(-38.9663238237679,54.927900505144,-448.85731067279));
#35802=CARTESIAN_POINT('Ctrl Pts',(-39.3072807059536,55.4140183332813,-448.166462398451));
#35803=CARTESIAN_POINT('Ctrl Pts',(-39.3076095549431,55.4144871883328,-448.16579608324));
#35804=CARTESIAN_POINT('Ctrl Pts',(-39.3079384041286,55.4149560434464,-448.165129767856));
#35805=CARTESIAN_POINT('Ctrl Pts',(-39.3082672535106,55.4154248986222,-448.164463452298));
#35806=CARTESIAN_POINT('Ctrl Pts',(-39.3211730900984,55.4338253232971,-448.138313609296));
#35807=CARTESIAN_POINT('Ctrl Pts',(-39.3340792292319,55.4522258436757,-448.11216349893));
#35808=CARTESIAN_POINT('Ctrl Pts',(-39.3469856562669,55.4706264654386,-448.086013119611));
#35809=CARTESIAN_POINT('Ctrl Pts',(-39.3630367564735,55.4935104303793,-448.053491155341));
#35810=CARTESIAN_POINT('Ctrl Pts',(-39.3790883019688,55.5163945521283,-448.020968775089));
#35811=CARTESIAN_POINT('Ctrl Pts',(-39.3951402645792,55.5392788416133,-447.988445975798));
#35812=CARTESIAN_POINT('Ctrl Pts',(-39.9518000701818,56.33287426949,-446.860600392663));
#35813=CARTESIAN_POINT('Ctrl Pts',(-40.5089619902815,57.1266713155322,-445.732251028844));
#35814=CARTESIAN_POINT('Ctrl Pts',(-41.0654476693404,57.9211264847329,-444.603269305596));
#35815=CARTESIAN_POINT('Ctrl Pts',(-41.068256646187,57.9251366619217,-444.597570536264));
#35816=CARTESIAN_POINT('Ctrl Pts',(-41.0710656057938,57.9291468558807,-444.591871750819));
#35817=CARTESIAN_POINT('Ctrl Pts',(-41.073874548009,57.9331570666687,-444.586172949239));
#35818=CARTESIAN_POINT('Ctrl Pts',(-41.0742819911305,57.9337387563854,-444.58534632579));
#35819=CARTESIAN_POINT('Ctrl Pts',(-41.074689433886,57.9343204464562,-444.584519702));
#35820=CARTESIAN_POINT('Ctrl Pts',(-41.0752464259017,57.9351156433501,-444.58338966975));
#35821=CARTESIAN_POINT('Ctrl Pts',(-41.0753959754787,57.9353291498666,-444.583086261584));
#35822=CARTESIAN_POINT('Ctrl Pts',(-41.6623439855686,58.7732940367474,-443.392277776917));
#35823=CARTESIAN_POINT('Ctrl Pts',(-42.2483816075473,59.6117803613952,-442.201068283792));
#35824=CARTESIAN_POINT('Ctrl Pts',(-42.8376428218466,60.4524075711013,-441.006506688383));
#35825=CARTESIAN_POINT('Ctrl Pts',(-42.8392516610929,60.4547026876939,-441.003245242575));
#35826=CARTESIAN_POINT('Ctrl Pts',(-42.876318266513,60.5075802484488,-440.928104213679));
#35827=CARTESIAN_POINT('Ctrl Pts',(-42.9117760205334,60.5581626937845,-440.856224631257));
#35828=CARTESIAN_POINT('Ctrl Pts',(-42.9472337745537,60.6087451391203,-440.784345048834));
#35829=CARTESIAN_POINT('Ctrl Pts',(-31.7948796623065,45.4225605594505,-462.499999999992));
#35830=CARTESIAN_POINT('Ctrl Pts',(-32.3588794542992,46.2684182687363,-461.305621084361));
#35831=CARTESIAN_POINT('Ctrl Pts',(-32.9228912587844,47.1142703716486,-460.111245917452));
#35832=CARTESIAN_POINT('Ctrl Pts',(-33.487095575851,47.960402219425,-458.916474195592));
#35833=CARTESIAN_POINT('Ctrl Pts',(-33.5108386678746,47.9960095086962,-458.866195291157));
#35834=CARTESIAN_POINT('Ctrl Pts',(-33.5345821010408,48.0316172932942,-458.815915684491));
#35835=CARTESIAN_POINT('Ctrl Pts',(-33.5583258888889,48.0672255944519,-458.765635345777));
#35836=CARTESIAN_POINT('Ctrl Pts',(-33.8315805468946,48.4770226418846,-458.186985601788));
#35837=CARTESIAN_POINT('Ctrl Pts',(-34.1048813488116,48.8868884209216,-457.608238733626));
#35838=CARTESIAN_POINT('Ctrl Pts',(-34.3782537048229,49.2968534751884,-457.029350268047));
#35839=CARTESIAN_POINT('Ctrl Pts',(-34.5132703451794,49.4993322667469,-456.743441418651));
#35840=CARTESIAN_POINT('Ctrl Pts',(-34.6483046294387,49.7018352029504,-456.457498067189));
#35841=CARTESIAN_POINT('Ctrl Pts',(-34.7833597254613,49.9043659276222,-456.171514872232));
#35842=CARTESIAN_POINT('Ctrl Pts',(-34.9151554033029,50.102008778044,-455.892433592512));
#35843=CARTESIAN_POINT('Ctrl Pts',(-35.0469709497132,50.2996780738909,-455.613314378314));
#35844=CARTESIAN_POINT('Ctrl Pts',(-35.1788083996885,50.4973775420912,-455.334152087623));
#35845=CARTESIAN_POINT('Ctrl Pts',(-35.3485792063683,50.7519607292116,-454.974666923932));
#35846=CARTESIAN_POINT('Ctrl Pts',(-35.5183862530979,51.0065939799953,-454.615110313089));
#35847=CARTESIAN_POINT('Ctrl Pts',(-35.6882312710722,51.2612862178016,-454.255470778925));
#35848=CARTESIAN_POINT('Ctrl Pts',(-36.0823826088463,51.8523385044639,-453.420872241992));
#35849=CARTESIAN_POINT('Ctrl Pts',(-36.4767353190538,52.4437095841588,-452.585826569913));
#35850=CARTESIAN_POINT('Ctrl Pts',(-36.87136162915,53.0354928881843,-451.750199183157));
#35851=CARTESIAN_POINT('Ctrl Pts',(-37.1087723710762,53.3915150531381,-451.247478222116));
#35852=CARTESIAN_POINT('Ctrl Pts',(-37.3462763440645,53.7476890875467,-450.744544962216));
#35853=CARTESIAN_POINT('Ctrl Pts',(-37.5838553593534,54.1039950517834,-450.241428853719));
#35854=CARTESIAN_POINT('Ctrl Pts',(-37.9099329633186,54.5930255958134,-449.550901136127));
#35855=CARTESIAN_POINT('Ctrl Pts',(-38.2362057805615,55.082285128756,-448.860038777299));
#35856=CARTESIAN_POINT('Ctrl Pts',(-38.5627017963575,55.5716951867403,-448.168931295036));
#35857=CARTESIAN_POINT('Ctrl Pts',(-38.5630166980077,55.5721672171096,-448.168264729822));
#35858=CARTESIAN_POINT('Ctrl Pts',(-38.5633315998594,55.5726392476211,-448.167598164379));
#35859=CARTESIAN_POINT('Ctrl Pts',(-38.5636465019127,55.5731112782746,-448.166931598707));
#35860=CARTESIAN_POINT('Ctrl Pts',(-38.5760049695387,55.5916363259503,-448.140771939877));
#35861=CARTESIAN_POINT('Ctrl Pts',(-38.5883637478265,55.6101615924535,-448.114611928373));
#35862=CARTESIAN_POINT('Ctrl Pts',(-38.6007228216992,55.6286870798237,-448.088451565684));
#35863=CARTESIAN_POINT('Ctrl Pts',(-38.616093205203,55.651726334092,-448.055917185578));
#35864=CARTESIAN_POINT('Ctrl Pts',(-38.6314640458791,55.6747659299684,-448.023382262304));
#35865=CARTESIAN_POINT('Ctrl Pts',(-38.6468353147218,55.6978058713774,-447.990846798726));
#35866=CARTESIAN_POINT('Ctrl Pts',(-39.1798896043096,56.4967990921528,-446.862562035657));
#35867=CARTESIAN_POINT('Ctrl Pts',(-39.7134592987254,57.2962077502379,-445.733627656976));
#35868=CARTESIAN_POINT('Ctrl Pts',(-40.2463313260584,58.0961962652654,-444.604161990745));
#35869=CARTESIAN_POINT('Ctrl Pts',(-40.2490211081019,58.1002343731646,-444.59846077861));
#35870=CARTESIAN_POINT('Ctrl Pts',(-40.2517108723597,58.1042724958398,-444.592759552937));
#35871=CARTESIAN_POINT('Ctrl Pts',(-40.2544006186752,58.1083106333122,-444.587058313738));
#35872=CARTESIAN_POINT('Ctrl Pts',(-40.2547907721747,58.1088963738547,-444.586231336706));
#35873=CARTESIAN_POINT('Ctrl Pts',(-40.2551809252966,58.1094821147085,-444.58540435939));
#35874=CARTESIAN_POINT('Ctrl Pts',(-40.2557142815918,58.1102828491458,-444.584273843927));
#35875=CARTESIAN_POINT('Ctrl Pts',(-40.2558574850924,58.1104978424598,-444.583970306028));
#35876=CARTESIAN_POINT('Ctrl Pts',(-40.817898576209,58.9542980499274,-443.392652678696));
#35877=CARTESIAN_POINT('Ctrl Pts',(-41.3790115672474,59.7985292162566,-442.201048219499));
#35878=CARTESIAN_POINT('Ctrl Pts',(-41.9432149726083,60.6444843430236,-441.006495234176));
#35879=CARTESIAN_POINT('Ctrl Pts',(-41.9447553974262,60.6467940028981,-441.003233814901));
#35880=CARTESIAN_POINT('Ctrl Pts',(-41.980245779804,60.7000065541704,-440.928093467114));
#35881=CARTESIAN_POINT('Ctrl Pts',(-42.0141957256967,60.7509094499825,-440.856214536236));
#35882=CARTESIAN_POINT('Ctrl Pts',(-42.0481456715894,60.8018123457946,-440.784335605358));
#35883=CARTESIAN_POINT('',(-56.601452649167,53.2766361680307,-440.999994148306));
#35884=CARTESIAN_POINT('Ctrl Pts',(-56.601452649167,53.2766361680307,-440.999994148306));
#35885=CARTESIAN_POINT('Ctrl Pts',(-54.7738391120521,52.0698384740113,-443.227191994004));
#35886=CARTESIAN_POINT('Ctrl Pts',(-53.3158598386457,51.107187317318,-445.003882932941));
#35887=CARTESIAN_POINT('Ctrl Pts',(-51.6833143334207,50.029459956972,-446.993158893569));
#35888=CARTESIAN_POINT('Ctrl Pts',(-51.0056480219981,49.582157997243,-447.818856763786));
#35889=CARTESIAN_POINT('Ctrl Pts',(-50.4575987060053,49.2205386069633,-448.486525753376));
#35890=CARTESIAN_POINT('Ctrl Pts',(-50.2442148715028,49.0797866305474,-448.746448951586));
#35891=CARTESIAN_POINT('Ctrl Pts',(-50.1400159078363,49.0110713760401,-448.873361284946));
#35892=CARTESIAN_POINT('Ctrl Pts',(-50.0938062106593,48.9806040828583,-448.929638990356));
#35893=CARTESIAN_POINT('Ctrl Pts',(-50.0719407184908,48.966189323167,-448.956267112864));
#35894=CARTESIAN_POINT('Ctrl Pts',(-50.0725610927088,48.9665983008579,-448.955511613539));
#35895=CARTESIAN_POINT('Ctrl Pts',(-49.7377894632215,48.7459020199295,-449.363200799079));
#35896=CARTESIAN_POINT('Ctrl Pts',(-49.4352278905934,48.5459054812786,-449.732078168407));
#35897=CARTESIAN_POINT('Ctrl Pts',(-49.0277940186024,48.275622186605,-450.229556155105));
#35898=CARTESIAN_POINT('Ctrl Pts',(-48.8356784662846,48.1479084645981,-450.464336151231));
#35899=CARTESIAN_POINT('Ctrl Pts',(-48.631853759036,48.0119009321817,-450.713817161894));
#35900=CARTESIAN_POINT('Ctrl Pts',(-48.5281028279955,47.9425189717714,-450.840924242818));
#35901=CARTESIAN_POINT('Ctrl Pts',(-48.4811669407684,47.9110877548734,-450.898459603619));
#35902=CARTESIAN_POINT('Ctrl Pts',(-48.4547091942354,47.89335897057,-450.930900721537));
#35903=CARTESIAN_POINT('Ctrl Pts',(-48.4493956713363,47.8897979200664,-450.93741632498));
#35904=CARTESIAN_POINT('Ctrl Pts',(-48.1911818927057,47.7167009016883,-451.254080950314));
#35905=CARTESIAN_POINT('Ctrl Pts',(-47.923909337161,47.5360147897983,-451.583018814021));
#35906=CARTESIAN_POINT('Ctrl Pts',(-47.6043364692148,47.3181959778586,-451.977676579559));
#35907=CARTESIAN_POINT('Ctrl Pts',(-47.5685660211511,47.2937918188525,-452.02186914582));
#35908=CARTESIAN_POINT('Ctrl Pts',(-47.4965008239971,47.2445789396727,-452.11093768424));
#35909=CARTESIAN_POINT('Ctrl Pts',(-47.4642724250937,47.2225555768963,-452.150781383843));
#35910=CARTESIAN_POINT('Ctrl Pts',(-47.3634872668974,47.1536731292441,-452.275388990803));
#35911=CARTESIAN_POINT('Ctrl Pts',(-47.1661706984304,47.0187276878275,-452.519410718903));
#35912=CARTESIAN_POINT('Ctrl Pts',(-46.969015806605,46.8836314119994,-452.763428011278));
#35913=CARTESIAN_POINT('Ctrl Pts',(-46.8348570128172,46.7915814454118,-452.929565431352));
#35914=CARTESIAN_POINT('Ctrl Pts',(-46.8316879630588,46.7894070127498,-452.933489914907));
#35915=CARTESIAN_POINT('Ctrl Pts',(-46.4926707116515,46.5567784766192,-453.353331356604));
#35916=CARTESIAN_POINT('Ctrl Pts',(-46.1908192095058,46.3511215126281,-453.726005587852));
#35917=CARTESIAN_POINT('Ctrl Pts',(-45.7857235243058,46.0779816977538,-454.223955146678));
#35918=CARTESIAN_POINT('Ctrl Pts',(-45.5950973931695,45.9502467837759,-454.457664487715));
#35919=CARTESIAN_POINT('Ctrl Pts',(-45.3935239240952,45.8167251802618,-454.703611002445));
#35920=CARTESIAN_POINT('Ctrl Pts',(-45.297939241582,45.7538440372232,-454.819905681308));
#35921=CARTESIAN_POINT('Ctrl Pts',(-45.2481260815286,45.7211974134129,-454.880417499361));
#35922=CARTESIAN_POINT('Ctrl Pts',(-45.2252590617721,45.7062454173416,-454.908169368993));
#35923=CARTESIAN_POINT('Ctrl Pts',(-45.2122850284238,45.6977707604777,-454.923908320153));
#35924=CARTESIAN_POINT('Ctrl Pts',(-45.2098033528762,45.696150112695,-454.926918574951));
#35925=CARTESIAN_POINT('Ctrl Pts',(-44.6961082429141,45.3608345902825,-455.549911919046));
#35926=CARTESIAN_POINT('Ctrl Pts',(-44.1419304533118,45.0135796250764,-456.210946793152));
#35927=CARTESIAN_POINT('Ctrl Pts',(-43.5419127712896,44.6532698807934,-456.914899800777));
#35928=CARTESIAN_POINT('Ctrl Pts',(-41.9462958339113,60.6491036583583,-440.999972397991));
#35929=CARTESIAN_POINT('Ctrl Pts',(-42.4536076986967,60.5401595182708,-440.999978861914));
#35930=CARTESIAN_POINT('Ctrl Pts',(-42.9582396954925,60.4191084556018,-441.000072725249));
#35931=CARTESIAN_POINT('Ctrl Pts',(-43.9613151855463,60.1529933426888,-441.000299642132));
#35932=CARTESIAN_POINT('Ctrl Pts',(-44.4596200480986,60.0079647356423,-441.000418945381));
#35933=CARTESIAN_POINT('Ctrl Pts',(-45.9432689217911,59.5374326211282,-441.000516453555));
#35934=CARTESIAN_POINT('Ctrl Pts',(-46.9167473739368,59.1766923215432,-441.000393081996));
#35935=CARTESIAN_POINT('Ctrl Pts',(-48.5073188404937,58.4992293403753,-441.000331534641));
#35936=CARTESIAN_POINT('Ctrl Pts',(-49.134498395159,58.2081810247175,-441.000338333599));
#35937=CARTESIAN_POINT('Ctrl Pts',(-50.986111138267,57.2761989420374,-441.000292512001));
#35938=CARTESIAN_POINT('Ctrl Pts',(-52.1794941815985,56.5771072599769,-441.000229810147));
#35939=CARTESIAN_POINT('Ctrl Pts',(-53.8971333256094,55.4182676375983,-441.000147690528));
#35940=CARTESIAN_POINT('Ctrl Pts',(-54.4569722800717,55.0140887402452,-441.000120670842));
#35941=CARTESIAN_POINT('Ctrl Pts',(-55.2767819376056,54.3816364844746,-441.000066623273));
#35942=CARTESIAN_POINT('Ctrl Pts',(-55.5466526868058,54.1665147681349,-441.000049725274));
#35943=CARTESIAN_POINT('Ctrl Pts',(-55.9462310386895,53.8374804277519,-441.000028586167));
#35944=CARTESIAN_POINT('Ctrl Pts',(-56.0785341359438,53.7267594825738,-441.000022093514));
#35945=CARTESIAN_POINT('Ctrl Pts',(-56.2756523821078,53.5591158372563,-441.000012193514));
#35946=CARTESIAN_POINT('Ctrl Pts',(-56.3411311310312,53.5029782684191,-441.000008857992));
#35947=CARTESIAN_POINT('Ctrl Pts',(-56.4390115504381,53.418384631197,-441.000003597922));
#35948=CARTESIAN_POINT('Ctrl Pts',(-56.4715809264883,53.39012321023,-441.000001801287));
#35949=CARTESIAN_POINT('Ctrl Pts',(-56.5437212175141,53.3272733766563,-440.999997673909));
#35950=CARTESIAN_POINT('Ctrl Pts',(-56.5769261061491,53.2981760183113,-440.999995669541));
#35951=CARTESIAN_POINT('Ctrl Pts',(-56.601452649167,53.2766361680308,-440.999994148306));
#35952=CARTESIAN_POINT('Ctrl Pts',(-64.2658958771365,45.6374763139969,-440.999637204112));
#35953=CARTESIAN_POINT('Ctrl Pts',(-55.774321890447,32.4272154387425,-456.914897282309));
#35954=CARTESIAN_POINT('Ctrl Pts',(-61.8717342174773,48.3453380510754,-440.999999999991));
#35955=CARTESIAN_POINT('Ctrl Pts',(-51.8201097042196,36.6236615680269,-456.919527670999));
#35956=CARTESIAN_POINT('Ctrl Pts',(-59.3135877730462,50.8952105744119,-440.999999999991));
#35957=CARTESIAN_POINT('Ctrl Pts',(-47.7405554577368,40.7010682615931,-456.919527671));
#35958=CARTESIAN_POINT('Ctrl Pts',(-56.601452649167,53.2766361680307,-440.999994148306));
#35959=CARTESIAN_POINT('Ctrl Pts',(-43.5418850322421,44.6532394081086,-456.91486065554));
#35960=CARTESIAN_POINT('Ctrl Pts',(-56.6012177920432,53.2768423873892,-440.999994147799));
#35961=CARTESIAN_POINT('Ctrl Pts',(-43.5415211446437,44.6535819322701,-456.914860251062));
#35962=CARTESIAN_POINT('Ctrl Pts',(-56.6009829349194,53.2770486067477,-440.999994147292));
#35963=CARTESIAN_POINT('Ctrl Pts',(-43.5411572570453,44.6539244564316,-456.914859846584));
#35964=CARTESIAN_POINT('Ctrl Pts',(-56.6007480777956,53.2772548261063,-440.999994146786));
#35965=CARTESIAN_POINT('Ctrl Pts',(-43.5407933694469,44.6542669805931,-456.914859442107));
#35966=CARTESIAN_POINT('',(-64.2657028580431,45.6371756443949,-440.999998037155));
#35967=CARTESIAN_POINT('',(-64.2657034184046,45.63717615959,-440.999998440138));
#35968=CARTESIAN_POINT('Ctrl Pts',(-56.601452649167,53.2766361680308,-440.999994148306));
#35969=CARTESIAN_POINT('Ctrl Pts',(-57.7028809440721,52.3093280492766,-441.000142795397));
#35970=CARTESIAN_POINT('Ctrl Pts',(-58.7792997824101,51.3139675750334,-441.000170909128));
#35971=CARTESIAN_POINT('Ctrl Pts',(-59.8294787290137,50.2917255855174,-441.00015198801));
#35972=CARTESIAN_POINT('Ctrl Pts',(-60.8795257991174,49.2696119643105,-441.000133069268));
#35973=CARTESIAN_POINT('Ctrl Pts',(-61.9033396129511,48.220623538411,-441.000067127489));
#35974=CARTESIAN_POINT('Ctrl Pts',(-62.8997269250625,47.1459676259387,-441.000027633498));
#35975=CARTESIAN_POINT('Ctrl Pts',(-63.3609673081903,46.6484957103752,-441.000009351227));
#35976=CARTESIAN_POINT('Ctrl Pts',(-63.8163310265106,46.1455240769036,-440.999996736404));
#35977=CARTESIAN_POINT('Ctrl Pts',(-64.2657023428471,45.6371752088159,-440.999997077097));
#35978=CARTESIAN_POINT('Ctrl Pts',(-69.7776904941909,32.0305578312519,-441.000027286454));
#35979=CARTESIAN_POINT('Ctrl Pts',(-56.5915605594688,20.6258796622837,-462.499999999988));
#35980=CARTESIAN_POINT('Ctrl Pts',(-69.5425906598027,37.113747189771,-440.99999999999));
#35981=CARTESIAN_POINT('Ctrl Pts',(-56.0041009291263,23.3343857139598,-462.499999999988));
#35982=CARTESIAN_POINT('Ctrl Pts',(-67.6327997693356,41.8281639590277,-440.99999999999));
#35983=CARTESIAN_POINT('Ctrl Pts',(-54.7064708585609,25.7833181444718,-462.499999999989));
#35984=CARTESIAN_POINT('Ctrl Pts',(-64.2658958771893,45.637476314079,-440.999637204013));
#35985=CARTESIAN_POINT('Ctrl Pts',(-52.7943871585138,27.7913593228122,-462.500014523132));
#35986=CARTESIAN_POINT('',(-69.7776893278308,32.0305568224675,-441.000029188202));
#35987=CARTESIAN_POINT('Origin',(-47.7274224530678,31.0176628730264,-440.980660458913));
#35988=CARTESIAN_POINT('Origin',(-54.2736315587492,-11.1690000000156,-438.999999999984));
#35989=CARTESIAN_POINT('',(-70.5084762417148,-34.7635952579923,-438.99999999998));
#35990=CARTESIAN_POINT('',(-70.4554509568028,-36.792411599386,-438.99999999998));
#35991=CARTESIAN_POINT('Origin',(871.003976208289,-11.171261467625,-438.999999999992));
#35992=CARTESIAN_POINT('Ctrl Pts',(-70.508476241715,-34.7635952579923,-438.999999999982));
#35993=CARTESIAN_POINT('Ctrl Pts',(-70.4767675684555,-35.1005664161786,
-438.999999999982));
#35994=CARTESIAN_POINT('Ctrl Pts',(-70.456475079011,-35.4385125585903,-438.999999999979));
#35995=CARTESIAN_POINT('Ctrl Pts',(-70.4387772188577,-36.1153666437888,
-438.999999999979));
#35996=CARTESIAN_POINT('Ctrl Pts',(-70.4413882261958,-36.45407804119,-438.999999999981));
#35997=CARTESIAN_POINT('Ctrl Pts',(-70.4554509568029,-36.7924115993857,
-438.999999999981));
#35998=CARTESIAN_POINT('Ctrl Pts',(-69.7814241414421,-54.3757509201429,
-440.993983453141));
#35999=CARTESIAN_POINT('Ctrl Pts',(-69.7777140088065,-54.3725409130246,
-441.000032808645));
#36000=CARTESIAN_POINT('Ctrl Pts',(-56.5915605594633,-42.9638796623204,
-462.499999999981));
#36001=CARTESIAN_POINT('Ctrl Pts',(-56.5783744060139,-42.9524710010697,
-462.521499967173));
#36002=CARTESIAN_POINT('Ctrl Pts',(-69.9806527515224,-49.9927595127392,
-440.993963941929));
#36003=CARTESIAN_POINT('Ctrl Pts',(-69.9770872889478,-49.9898995318794,
-440.99999999998));
#36004=CARTESIAN_POINT('Ctrl Pts',(-57.277168782509,-39.8028556101424,-462.499999999981));
#36005=CARTESIAN_POINT('Ctrl Pts',(-57.2644408666255,-39.792646108556,-462.52154739742));
#36006=CARTESIAN_POINT('Ctrl Pts',(-70.1511013536826,-45.6102732255524,
-440.993975224971));
#36007=CARTESIAN_POINT('Ctrl Pts',(-70.1476583281878,-45.6077541556496,
-440.99999999998));
#36008=CARTESIAN_POINT('Ctrl Pts',(-57.8608844602732,-36.6182063587309,
-462.499999999982));
#36009=CARTESIAN_POINT('Ctrl Pts',(-57.8485475387398,-36.6091801206816,
-462.521587750828));
#36010=CARTESIAN_POINT('Ctrl Pts',(-70.2928114147138,-41.2265701727283,
-440.994016766951));
#36011=CARTESIAN_POINT('Ctrl Pts',(-70.2894684716153,-41.2243846605893,
-441.000032274629));
#36012=CARTESIAN_POINT('Ctrl Pts',(-58.341487923045,-33.4131668933052,-462.499999999982));
#36013=CARTESIAN_POINT('Ctrl Pts',(-58.3294727137636,-33.4053117234853,
-462.521620943431));
#36014=CARTESIAN_POINT('',(-70.2893406259791,-41.2283906269187,-441.000029101383));
#36015=CARTESIAN_POINT('Ctrl Pts',(-70.2893406186478,-41.228390626661,-441.000029070991));
#36016=CARTESIAN_POINT('Ctrl Pts',(-70.1494588909743,-45.6109060280408,
-440.996616656315));
#36017=CARTESIAN_POINT('Ctrl Pts',(-69.9789058201507,-49.992411625971,-440.996967909007));
#36018=CARTESIAN_POINT('Ctrl Pts',(-69.7777140088065,-54.3725409130246,
-441.000032808645));
#36019=CARTESIAN_POINT('Ctrl Pts',(-70.2893406401635,-41.2283906506288,
-441.000029112448));
#36020=CARTESIAN_POINT('Ctrl Pts',(-69.123590435456,-40.9599833732949,-443.069542538055));
#36021=CARTESIAN_POINT('Ctrl Pts',(-67.9450458275156,-40.6639886984268,
-445.141170812192));
#36022=CARTESIAN_POINT('Ctrl Pts',(-65.551152303873,-40.004777240294,-449.304140893811));
#36023=CARTESIAN_POINT('Ctrl Pts',(-64.3222984007391,-39.6362874672872,
-451.417506435825));
#36024=CARTESIAN_POINT('Ctrl Pts',(-61.3238515421179,-38.6439304718567,
-456.517206904405));
#36025=CARTESIAN_POINT('Ctrl Pts',(-59.5048995836444,-37.9635263279722,
-459.558563915027));
#36026=CARTESIAN_POINT('Ctrl Pts',(-57.7295804999056,-37.1684431733089,
-462.499999999981));
#36027=CARTESIAN_POINT('Ctrl Pts',(-70.292529859086,18.8884758131824,-440.994261297969));
#36028=CARTESIAN_POINT('Ctrl Pts',(-70.2893242457657,18.886380058914,-441.000029755883));
#36029=CARTESIAN_POINT('Ctrl Pts',(-58.3414879230488,11.0751668932692,-462.499999999987));
#36030=CARTESIAN_POINT('Ctrl Pts',(-58.3294728588049,11.0673117280768,-462.521620945969));
#36031=CARTESIAN_POINT('Ctrl Pts',(-70.15095995233,23.2721697700229,-440.994222656018));
#36032=CARTESIAN_POINT('Ctrl Pts',(-70.1476583281939,23.2697541556153,-440.999999999988));
#36033=CARTESIAN_POINT('Ctrl Pts',(-57.8608844602774,14.2802063586947,-462.499999999988));
#36034=CARTESIAN_POINT('Ctrl Pts',(-57.8485475387442,14.2711801206454,-462.521587750834));
#36035=CARTESIAN_POINT('Ctrl Pts',(-69.9805063218111,27.6546420563625,-440.994211836358));
#36036=CARTESIAN_POINT('Ctrl Pts',(-69.9770872889547,27.6518995318446,-440.999999999989));
#36037=CARTESIAN_POINT('Ctrl Pts',(-57.277168782514,17.4648556101059,-462.499999999988));
#36038=CARTESIAN_POINT('Ctrl Pts',(-57.2644408666304,17.4546461085195,-462.521547397427));
#36039=CARTESIAN_POINT('Ctrl Pts',(-69.7812482493198,32.0336349321488,-440.994226369993));
#36040=CARTESIAN_POINT('Ctrl Pts',(-69.7776904941909,32.0305578312519,-441.000027286454));
#36041=CARTESIAN_POINT('Ctrl Pts',(-56.5915605594688,20.6258796622837,-462.499999999988));
#36042=CARTESIAN_POINT('Ctrl Pts',(-56.5783744295341,20.6144749841147,-462.521499972702));
#36043=CARTESIAN_POINT('',(-70.289206435783,18.8900706285948,-441.000027137208));
#36044=CARTESIAN_POINT('Ctrl Pts',(-57.7295804999102,14.8304431732719,-462.499999999987));
#36045=CARTESIAN_POINT('Ctrl Pts',(-59.5045045244752,15.6253388507935,-459.559205212572));
#36046=CARTESIAN_POINT('Ctrl Pts',(-61.3230116147034,16.3055894393686,-456.518594345998));
#36047=CARTESIAN_POINT('Ctrl Pts',(-64.3212741457954,17.2978938106733,-451.419209339214));
#36048=CARTESIAN_POINT('Ctrl Pts',(-65.550328672081,17.6664301595495,-449.305489097914));
#36049=CARTESIAN_POINT('Ctrl Pts',(-67.9445832191676,18.3256861822974,-445.141842101897));
#36050=CARTESIAN_POINT('Ctrl Pts',(-69.1233006778753,18.6216836058714,-443.069871435287));
#36051=CARTESIAN_POINT('Ctrl Pts',(-70.2892064356818,18.8900706273276,-441.000027136986));
#36052=CARTESIAN_POINT('Ctrl Pts',(-69.7776893278306,32.0305568224675,-441.000029188203));
#36053=CARTESIAN_POINT('Ctrl Pts',(-69.8782554180672,29.8411055079886,-440.998663142711));
#36054=CARTESIAN_POINT('Ctrl Pts',(-69.9711674064275,27.6513214514411,-440.997879764828));
#36055=CARTESIAN_POINT('Ctrl Pts',(-70.1416774153024,23.2710915157206,-440.997783805102));
#36056=CARTESIAN_POINT('Ctrl Pts',(-70.2192715819682,21.0807504505387,-440.99847273527));
#36057=CARTESIAN_POINT('Ctrl Pts',(-70.289206435962,18.8900706286,-441.00002713642));
#36058=CARTESIAN_POINT('Origin',(-54.2736315587492,-11.1690000000156,-438.999999999984));
#36059=CARTESIAN_POINT('',(-70.4553279483522,14.4544082600061,-438.999999999986));
#36060=CARTESIAN_POINT('',(-70.508362966475,12.4255924277826,-438.999999999986));
#36061=CARTESIAN_POINT('Origin',(871.003976208289,-11.171261467625,-438.999999999992));
#36062=CARTESIAN_POINT('Origin',(-85.4463381859629,13.8311852560246,-439.000015674809));
#36063=CARTESIAN_POINT('Ctrl Pts',(-58.3152526335012,7.11256737780218,-462.499999999986));
#36064=CARTESIAN_POINT('Ctrl Pts',(-70.9880999661371,9.82056904889893,-439.000749857024));
#36065=CARTESIAN_POINT('Ctrl Pts',(-57.2363227355981,9.63550019499528,-462.499999999987));
#36066=CARTESIAN_POINT('Ctrl Pts',(-70.1268305119616,12.9271295702052,-438.999052441603));
#36067=CARTESIAN_POINT('Ctrl Pts',(-57.0028527815747,12.4931127438228,-462.499999999987));
#36068=CARTESIAN_POINT('Ctrl Pts',(-70.2442207404255,16.2699753471456,-439.000717531333));
#36069=CARTESIAN_POINT('Ctrl Pts',(-57.8729593028357,15.3392709969105,-462.499999999987));
#36070=CARTESIAN_POINT('Ctrl Pts',(-71.5424551395504,19.4736999487602,-438.999999999988));
#36071=CARTESIAN_POINT('Ctrl Pts',(-70.2892064359492,18.8900706285019,-441.00002713733));
#36072=CARTESIAN_POINT('Ctrl Pts',(-70.3185646663934,18.2566939697067,-440.477202905431));
#36073=CARTESIAN_POINT('Ctrl Pts',(-70.347804124619,17.5655437203867,-440.030299535459));
#36074=CARTESIAN_POINT('Ctrl Pts',(-70.4043926371724,16.0677660576806,-439.340085108649));
#36075=CARTESIAN_POINT('Ctrl Pts',(-70.4311133436359,15.2759782175062,-439.106074007436));
#36076=CARTESIAN_POINT('Ctrl Pts',(-70.4553279483522,14.454408260006,-438.999999999988));
#36077=CARTESIAN_POINT('',(-70.5581573682015,9.72869661935509,-439.797992054518));
#36078=CARTESIAN_POINT('',(-58.3152526335012,7.11256737780218,-462.499999999987));
#36079=CARTESIAN_POINT('Ctrl Pts',(-70.5083629664747,12.4255924277829,-438.999999999988));
#36080=CARTESIAN_POINT('Ctrl Pts',(-70.5190417311927,11.9581189779784,-439.059413282611));
#36081=CARTESIAN_POINT('Ctrl Pts',(-70.528502917745,11.4975517735212,-439.158641883047));
#36082=CARTESIAN_POINT('Ctrl Pts',(-70.5450909658798,10.5948954496699,-439.428499909191));
#36083=CARTESIAN_POINT('Ctrl Pts',(-70.5521753927515,10.1552367203658,-439.59832946049));
#36084=CARTESIAN_POINT('Ctrl Pts',(-70.5581573682015,9.72869661935604,-439.797992054519));
#36085=CARTESIAN_POINT('Ctrl Pts',(-59.0902650976014,-0.703506953312267,
-462.499999999985));
#36086=CARTESIAN_POINT('Ctrl Pts',(-70.7677853055098,1.15015641282444,-439.798680793982));
#36087=CARTESIAN_POINT('Ctrl Pts',(-59.6440060900478,1.94053476148597,-462.499999999986));
#36088=CARTESIAN_POINT('Ctrl Pts',(-71.4248025866691,3.99812226801711,-439.789824991756));
#36089=CARTESIAN_POINT('Ctrl Pts',(-59.3774521833115,4.62875623508382,-462.499999999986));
#36090=CARTESIAN_POINT('Ctrl Pts',(-71.3533291948978,6.91847187716548,-439.789824991757));
#36091=CARTESIAN_POINT('Ctrl Pts',(-58.3152526335012,7.11256737780218,-462.499999999986));
#36092=CARTESIAN_POINT('Ctrl Pts',(-70.5581573682015,9.72869661935526,-439.797992054521));
#36093=CARTESIAN_POINT('',(-70.707553625092,1.14059537096935,-439.915772315053));
#36094=CARTESIAN_POINT('',(-59.0902650976014,-0.703506953312267,-462.499999999986));
#36095=CARTESIAN_POINT('Ctrl Pts',(-70.5581573682015,9.7286966193551,-439.797992054521));
#36096=CARTESIAN_POINT('Ctrl Pts',(-70.5678046345493,9.04133438885232,-440.119320391241));
#36097=CARTESIAN_POINT('Ctrl Pts',(-70.5782199854561,8.32772296577743,-440.386730380512));
#36098=CARTESIAN_POINT('Ctrl Pts',(-70.6003622288596,6.88955219928298,-440.760094435853));
#36099=CARTESIAN_POINT('Ctrl Pts',(-70.6119275337347,6.17248248578738,-440.870819207139));
#36100=CARTESIAN_POINT('Ctrl Pts',(-70.637063876889,4.7026944634276,-440.916714503241));
#36101=CARTESIAN_POINT('Ctrl Pts',(-70.6503587134966,3.96810546432371,-440.847278158492));
#36102=CARTESIAN_POINT('Ctrl Pts',(-70.6784620794615,2.5112022870367,-440.514928775699));
#36103=CARTESIAN_POINT('Ctrl Pts',(-70.6928736353993,1.81053750859871,-440.254969959199));
#36104=CARTESIAN_POINT('Ctrl Pts',(-70.707553625092,1.14059537097008,-439.915772315053));
#36105=CARTESIAN_POINT('Origin',(-54.2736315587492,-11.1690000000156,-438.999999999984));
#36106=CARTESIAN_POINT('',(-70.7571158415876,-1.77222784066373,-438.999999999984));
#36107=CARTESIAN_POINT('',(-70.776418222841,-3.96119924583428,-438.999999999984));
#36108=CARTESIAN_POINT('Origin',(871.003976208289,-11.171261467625,-438.999999999992));
#36109=CARTESIAN_POINT('Ctrl Pts',(-70.7571158415876,-1.77222784066382,
-438.999999999986));
#36110=CARTESIAN_POINT('Ctrl Pts',(-70.7374577456278,-2.13718693330326,
-438.999999999986));
#36111=CARTESIAN_POINT('Ctrl Pts',(-70.7292454393531,-2.50266922432743,
-438.999999999985));
#36112=CARTESIAN_POINT('Ctrl Pts',(-70.7357313681723,-3.23286508272366,
-438.999999999985));
#36113=CARTESIAN_POINT('Ctrl Pts',(-70.7503808772078,-3.59739324964435,
-438.999999999986));
#36114=CARTESIAN_POINT('Ctrl Pts',(-70.7764182228409,-3.96119924583425,
-438.999999999986));
#36115=CARTESIAN_POINT('Ctrl Pts',(-59.4064050032667,-7.27543664707476,
-462.499999999985));
#36116=CARTESIAN_POINT('Ctrl Pts',(-71.2501735645804,-6.94091182239155,
-439.000746326908));
#36117=CARTESIAN_POINT('Ctrl Pts',(-58.7385280596105,-5.1359471967354,-462.499999999985));
#36118=CARTESIAN_POINT('Ctrl Pts',(-70.5811457040036,-4.25282607367328,
-438.999669295073));
#36119=CARTESIAN_POINT('Ctrl Pts',(-58.6308352736725,-2.89722502017172,
-462.499999999985));
#36120=CARTESIAN_POINT('Ctrl Pts',(-70.5567348878677,-1.48408888094075,
-438.999671718532));
#36121=CARTESIAN_POINT('Ctrl Pts',(-59.0902650976014,-0.703506953312267,
-462.499999999985));
#36122=CARTESIAN_POINT('Ctrl Pts',(-71.1782425626859,1.21531147720845,-439.000744155921));
#36123=CARTESIAN_POINT('',(-70.7782178075338,-6.95424211600733,-439.93715503818));
#36124=CARTESIAN_POINT('',(-59.4064050032667,-7.27543664707476,-462.499999999985));
#36125=CARTESIAN_POINT('Ctrl Pts',(-70.7764182228408,-3.96119924583428,
-438.999999999986));
#36126=CARTESIAN_POINT('Ctrl Pts',(-70.7792259582827,-4.48285116764463,
-439.067939102373));
#36127=CARTESIAN_POINT('Ctrl Pts',(-70.7807027348374,-4.99571525392328,
-439.183374598125));
#36128=CARTESIAN_POINT('Ctrl Pts',(-70.7812087649267,-5.99846114666605,
-439.500477515119));
#36129=CARTESIAN_POINT('Ctrl Pts',(-70.7802394325318,-6.48469492714696,
-439.700886889843));
#36130=CARTESIAN_POINT('Ctrl Pts',(-70.7782178073704,-6.95424211587693,
-439.937155038438));
#36131=CARTESIAN_POINT('Ctrl Pts',(-70.707553625092,1.14059537096959,-439.915772315052));
#36132=CARTESIAN_POINT('Ctrl Pts',(-70.7175664400768,0.684205669526496,
-439.683996098304));
#36133=CARTESIAN_POINT('Ctrl Pts',(-70.7268359140479,0.21125137401857,-439.488172163492));
#36134=CARTESIAN_POINT('Ctrl Pts',(-70.7435314502,-0.76501779240385,-439.178742173232));
#36135=CARTESIAN_POINT('Ctrl Pts',(-70.7508854143187,-1.26427873052628,
-439.066507814377));
#36136=CARTESIAN_POINT('Ctrl Pts',(-70.7571158415874,-1.77222784066387,
-438.999999999986));
#36137=CARTESIAN_POINT('Ctrl Pts',(-59.4064050032661,-15.0625633529625,
-462.499999999984));
#36138=CARTESIAN_POINT('Ctrl Pts',(-70.7782380423279,-15.3837579656666,
-439.937155391899));
#36139=CARTESIAN_POINT('Ctrl Pts',(-60.204044757482,-12.5073892965367,-462.499999999984));
#36140=CARTESIAN_POINT('Ctrl Pts',(-71.4803706009381,-12.6028580262609,
-439.927462314947));
#36141=CARTESIAN_POINT('Ctrl Pts',(-60.2040447574823,-9.83061070350056,
-462.499999999985));
#36142=CARTESIAN_POINT('Ctrl Pts',(-71.4803706009383,-9.73514197377313,
-439.927462314947));
#36143=CARTESIAN_POINT('Ctrl Pts',(-59.4064050032667,-7.27543664707476,
-462.499999999985));
#36144=CARTESIAN_POINT('Ctrl Pts',(-70.7782178073682,-6.95424211638727,
-439.937155038694));
#36145=CARTESIAN_POINT('',(-70.7782380423279,-15.3837579656666,-439.9371553919));
#36146=CARTESIAN_POINT('',(-59.4064050032661,-15.0625633529624,-462.499999999984));
#36147=CARTESIAN_POINT('Ctrl Pts',(-70.7782178073682,-6.95424211638724,
-439.937155038694));
#36148=CARTESIAN_POINT('Ctrl Pts',(-70.7753632379763,-7.61931765885983,
-440.271299916673));
#36149=CARTESIAN_POINT('Ctrl Pts',(-70.773068988079,-8.31344450348613,-440.540438931827));
#36150=CARTESIAN_POINT('Ctrl Pts',(-70.7699981011486,-9.73451302894079,
-440.901051397528));
#36151=CARTESIAN_POINT('Ctrl Pts',(-70.7692082793061,-10.4455629420233,
-440.994026431782));
#36152=CARTESIAN_POINT('Ctrl Pts',(-70.7692093849802,-11.88970116692,-440.99430585424));
#36153=CARTESIAN_POINT('Ctrl Pts',(-70.7700014883587,-12.6013038302797,
-440.901465936896));
#36154=CARTESIAN_POINT('Ctrl Pts',(-70.7730793305623,-14.0235098939738,
-440.540838886405));
#36155=CARTESIAN_POINT('Ctrl Pts',(-70.7753781859942,-14.7181790435964,
-440.271549168403));
#36156=CARTESIAN_POINT('Ctrl Pts',(-70.7782380423279,-15.3837579656657,
-439.9371553919));
#36157=CARTESIAN_POINT('Origin',(-54.2736315587492,-11.1690000000156,-438.999999999984));
#36158=CARTESIAN_POINT('',(-70.7764528366089,-18.3768010105731,-438.999999999982));
#36159=CARTESIAN_POINT('',(-70.7571609664515,-20.5657726010771,-438.999999999982));
#36160=CARTESIAN_POINT('Origin',(871.003976208289,-11.171261467625,-438.999999999992));
#36161=CARTESIAN_POINT('Ctrl Pts',(-70.7764528366089,-18.3768010105731,
-438.999999999984));
#36162=CARTESIAN_POINT('Ctrl Pts',(-70.7503902427032,-18.7409820044107,
-438.999999999984));
#36163=CARTESIAN_POINT('Ctrl Pts',(-70.7357390480042,-19.1058864417604,
-438.999999999983));
#36164=CARTESIAN_POINT('Ctrl Pts',(-70.729303684327,-19.8360828380082,-438.999999999983));
#36165=CARTESIAN_POINT('Ctrl Pts',(-70.7375211543362,-20.2011888207014,
-438.999999999984));
#36166=CARTESIAN_POINT('Ctrl Pts',(-70.7571609664516,-20.5657726010769,
-438.999999999984));
#36167=CARTESIAN_POINT('Ctrl Pts',(-59.0902650975996,-21.634493046725,-462.499999999983));
#36168=CARTESIAN_POINT('Ctrl Pts',(-71.1782916618887,-23.5533103055587,
-439.000769312961));
#36169=CARTESIAN_POINT('Ctrl Pts',(-58.6308352736711,-19.4407749798654,
-462.499999999984));
#36170=CARTESIAN_POINT('Ctrl Pts',(-70.5567881485483,-20.8539012598249,
-438.999654953635));
#36171=CARTESIAN_POINT('Ctrl Pts',(-58.7385280596094,-17.2020528033017,
-462.499999999984));
#36172=CARTESIAN_POINT('Ctrl Pts',(-70.5811778706299,-18.0851841799639,
-438.999671159419));
#36173=CARTESIAN_POINT('Ctrl Pts',(-59.4064050032661,-15.0625633529625,
-462.499999999984));
#36174=CARTESIAN_POINT('Ctrl Pts',(-71.2501905188668,-15.3970881466845,
-439.000754870191));
#36175=CARTESIAN_POINT('',(-70.7076127187097,-23.4785961349091,-439.915773346617));
#36176=CARTESIAN_POINT('',(-59.0902650975996,-21.6344930467249,-462.499999999983));
#36177=CARTESIAN_POINT('Ctrl Pts',(-70.7571609664513,-20.5657726010769,
-438.999999999984));
#36178=CARTESIAN_POINT('Ctrl Pts',(-70.7509329724109,-21.0737218053046,
-439.066508123017));
#36179=CARTESIAN_POINT('Ctrl Pts',(-70.7435813995415,-21.5729826180562,
-439.178742939681));
#36180=CARTESIAN_POINT('Ctrl Pts',(-70.7268905415287,-22.5492518033819,
-439.488173552908));
#36181=CARTESIAN_POINT('Ctrl Pts',(-70.7176233372533,-23.0222061235976,
-439.68399760213));
#36182=CARTESIAN_POINT('Ctrl Pts',(-70.7076127187097,-23.4785961349081,
-439.915773346618));
#36183=CARTESIAN_POINT('Ctrl Pts',(-70.7782380423279,-15.3837579656662,
-439.937155391899));
#36184=CARTESIAN_POINT('Ctrl Pts',(-70.7802619096142,-15.8533053674025,
-439.700887922278));
#36185=CARTESIAN_POINT('Ctrl Pts',(-70.781233575539,-16.3395391453776,-439.500478619951));
#36186=CARTESIAN_POINT('Ctrl Pts',(-70.7807323681793,-17.3422849482419,
-439.18337532313));
#36187=CARTESIAN_POINT('Ctrl Pts',(-70.7792580624525,-17.8551489817955,
-439.067939400421));
#36188=CARTESIAN_POINT('Ctrl Pts',(-70.7764528366087,-18.3768010105732,
-438.999999999984));
#36189=CARTESIAN_POINT('Ctrl Pts',(-58.315252633498,-29.4505673778391,-462.499999999982));
#36190=CARTESIAN_POINT('Ctrl Pts',(-70.5582576736305,-32.0666988371032,
-439.797993805781));
#36191=CARTESIAN_POINT('Ctrl Pts',(-59.3774521833087,-26.966756235121,-462.499999999982));
#36192=CARTESIAN_POINT('Ctrl Pts',(-71.3533291948944,-29.2564718771995,
-439.789824991752));
#36193=CARTESIAN_POINT('Ctrl Pts',(-59.6440060900456,-24.2785347615233,
-462.499999999982));
#36194=CARTESIAN_POINT('Ctrl Pts',(-71.4248025866663,-26.3361222680511,
-439.789824991753));
#36195=CARTESIAN_POINT('Ctrl Pts',(-59.0902650975996,-21.634493046725,-462.499999999983));
#36196=CARTESIAN_POINT('Ctrl Pts',(-70.7678327375085,-23.4881552809602,
-439.798705096793));
#36197=CARTESIAN_POINT('',(-70.5582576736306,-32.0666988371032,-439.79799380578));
#36198=CARTESIAN_POINT('',(-58.315252633498,-29.4505673778391,-462.499999999982));
#36199=CARTESIAN_POINT('Ctrl Pts',(-70.7076127187096,-23.4785961349083,
-439.915773346619));
#36200=CARTESIAN_POINT('Ctrl Pts',(-70.692931806569,-24.1487583902344,-440.255043384189));
#36201=CARTESIAN_POINT('Ctrl Pts',(-70.6785197101522,-24.8496535886884,
-440.515026634784));
#36202=CARTESIAN_POINT('Ctrl Pts',(-70.6504156840113,-26.3070483489971,
-440.847322448924));
#36203=CARTESIAN_POINT('Ctrl Pts',(-70.6371209616,-27.0418804194973,-440.916677181194));
#36204=CARTESIAN_POINT('Ctrl Pts',(-70.6119935199245,-28.5116679207172,
-440.870550005376));
#36205=CARTESIAN_POINT('Ctrl Pts',(-70.6004358519606,-29.2285024225826,
-440.759792257379));
#36206=CARTESIAN_POINT('Ctrl Pts',(-70.5783080855848,-30.6661840163611,
-440.386490214465));
#36207=CARTESIAN_POINT('Ctrl Pts',(-70.5678992612722,-31.379554830566,-440.119180932133));
#36208=CARTESIAN_POINT('Ctrl Pts',(-70.5582576736304,-32.0666988371033,
-439.797993805781));
#36209=CARTESIAN_POINT('Ctrl Pts',(-57.8729592854352,-37.6772709400444,
-462.499999999981));
#36210=CARTESIAN_POINT('Ctrl Pts',(-71.5424551136841,-41.8116998850977,
-438.999999999981));
#36211=CARTESIAN_POINT('Ctrl Pts',(-57.002852784825,-34.8311127040267,-462.499999999982));
#36212=CARTESIAN_POINT('Ctrl Pts',(-70.2444010733898,-38.6079211063178,
-439.000759209165));
#36213=CARTESIAN_POINT('Ctrl Pts',(-57.2363227433805,-31.9735001768253,
-462.499999999982));
#36214=CARTESIAN_POINT('Ctrl Pts',(-70.1269516413443,-35.2651683193791,
-438.998997400818));
#36215=CARTESIAN_POINT('Ctrl Pts',(-58.315252633498,-29.4505673778391,-462.499999999982));
#36216=CARTESIAN_POINT('Ctrl Pts',(-70.9881812819792,-32.1585665340612,
-439.000793413576));
#36217=CARTESIAN_POINT('Ctrl Pts',(-70.4554509568026,-36.7924115993857,
-438.999999999982));
#36218=CARTESIAN_POINT('Ctrl Pts',(-70.4314005258243,-37.6085426071128,
-439.105374792254));
#36219=CARTESIAN_POINT('Ctrl Pts',(-70.404873950049,-38.395408212837,-439.336981328181));
#36220=CARTESIAN_POINT('Ctrl Pts',(-70.3483212379187,-39.8946310210821,
-440.024425265895));
#36221=CARTESIAN_POINT('Ctrl Pts',(-70.3188922841445,-40.590758615142,-440.473747059951));
#36222=CARTESIAN_POINT('Ctrl Pts',(-70.2893406183184,-41.2283906081489,
-441.000029123694));
#36223=CARTESIAN_POINT('Ctrl Pts',(-70.5582576736304,-32.0666988371036,
-439.797993805781));
#36224=CARTESIAN_POINT('Ctrl Pts',(-70.5522778094327,-32.4932382706619,
-439.598328470635));
#36225=CARTESIAN_POINT('Ctrl Pts',(-70.5451955315253,-32.9328963563196,
-439.428497688943));
#36226=CARTESIAN_POINT('Ctrl Pts',(-70.5286110764291,-33.8355932537874,
-439.1586274275));
#36227=CARTESIAN_POINT('Ctrl Pts',(-70.519152260206,-34.2961448342265,-439.059408910764));
#36228=CARTESIAN_POINT('Ctrl Pts',(-70.5084762417147,-34.7635952579922,
-438.999999999982));
#36229=CARTESIAN_POINT('Origin',(-1.50000000000897,104.331,-355.5));
#36230=CARTESIAN_POINT('',(-51.000000000009,104.330999999988,-407.5));
#36231=CARTESIAN_POINT('',(47.999999999991,104.330999999997,-407.5));
#36232=CARTESIAN_POINT('',(-1.500000000009,104.330999999993,-407.5));
#36233=CARTESIAN_POINT('',(-55.000000000009,104.330999999989,-403.5));
#36234=CARTESIAN_POINT('Origin',(-51.000000000009,104.330999999989,-403.5));
#36235=CARTESIAN_POINT('',(-55.000000000009,104.331,-307.5));
#36236=CARTESIAN_POINT('',(-55.000000000009,104.330999999994,-355.5));
#36237=CARTESIAN_POINT('',(-51.000000000009,104.331,-303.5));
#36238=CARTESIAN_POINT('Origin',(-51.000000000009,104.331,-307.5));
#36239=CARTESIAN_POINT('',(47.999999999991,104.331000000009,-303.5));
#36240=CARTESIAN_POINT('',(-25.500000000009,104.331000000003,-303.5));
#36241=CARTESIAN_POINT('',(51.999999999991,104.331000000009,-307.5));
#36242=CARTESIAN_POINT('Origin',(47.999999999991,104.331000000009,-307.5));
#36243=CARTESIAN_POINT('',(51.999999999991,104.330999999998,-403.5));
#36244=CARTESIAN_POINT('',(51.999999999991,104.331000000003,-355.5));
#36245=CARTESIAN_POINT('Origin',(47.999999999991,104.330999999998,-403.5));
#36246=CARTESIAN_POINT('Origin',(-47.7278656583192,-53.3599981836911,-427.99999999998));
#36247=CARTESIAN_POINT('',(-70.0043915535533,-54.382950086646,-427.999999999977));
#36248=CARTESIAN_POINT('',(-64.4357425873311,-68.1294560302671,-427.999999999978));
#36249=CARTESIAN_POINT('Origin',(-47.7278656583192,-53.3599981836911,-427.99999999998));
#36250=CARTESIAN_POINT('',(-70.004392491464,-54.3829501297155,-427.999946210488));
#36251=CARTESIAN_POINT('',(-64.4357419744368,-68.1294554884797,-428.000046864887));
#36252=CARTESIAN_POINT('Origin',(-0.00177950443039366,-11.1710102813481,
-427.999999999985));
#36253=CARTESIAN_POINT('',(-56.9487785810004,-75.6150902024262,-427.999999999977));
#36254=CARTESIAN_POINT('Origin',(-0.00177950443039366,-11.1710102813481,
-427.999999999985));
#36255=CARTESIAN_POINT('',(-56.9487778856762,-75.6150894155625,-428.000060157994));
#36256=CARTESIAN_POINT('Origin',(-42.1822887306986,-58.9045897810235,-427.99999999998));
#36257=CARTESIAN_POINT('',(-43.2050881469284,-81.1811229086658,-427.999999999976));
#36258=CARTESIAN_POINT('Origin',(-42.1822887306986,-58.9045897810235,-427.99999999998));
#36259=CARTESIAN_POINT('',(-43.2050880985635,-81.1811218552779,-428.0000604121));
#36260=CARTESIAN_POINT('Origin',(0.000158749880824205,859.827542634463,
-428.000000000085));
#36261=CARTESIAN_POINT('',(43.2079320035479,-81.1810069107222,-427.999999999977));
#36262=CARTESIAN_POINT('',(43.207931941457,-81.1810055584643,-428.000077552408));
#36263=CARTESIAN_POINT('Origin',(0.000158749880824205,859.827542634463,
-428.000000000083));
#36264=CARTESIAN_POINT('Origin',(42.1850727668518,-58.9044762258028,-427.999999999981));
#36265=CARTESIAN_POINT('',(56.9519860533863,-75.6146028669214,-427.999999999979));
#36266=CARTESIAN_POINT('Origin',(42.1850727668518,-58.9044762258028,-427.999999999981));
#36267=CARTESIAN_POINT('',(56.9519851501412,-75.614601844816,-428.000078144642));
#36268=CARTESIAN_POINT('Origin',(0.00335440791734976,-11.1719648985687,
-427.999999999985));
#36269=CARTESIAN_POINT('',(64.4405276263421,-68.1267798155728,-427.99999999998));
#36270=CARTESIAN_POINT('Origin',(0.00335440791734976,-11.1719648985687,
-427.999999999984));
#36271=CARTESIAN_POINT('',(64.4405263142287,-68.1267786558203,-428.000100325606));
#36272=CARTESIAN_POINT('Origin',(47.7318177098118,-53.3582629290221,-427.999999999981));
#36273=CARTESIAN_POINT('Origin',(47.7318177098118,-53.3582629290221,-427.999999999981));
#36274=CARTESIAN_POINT('Origin',(47.7318177098045,31.0202629290117,-427.999999999991));
#36275=CARTESIAN_POINT('',(64.4405276263324,45.7887798155652,-427.999999999993));
#36276=CARTESIAN_POINT('Origin',(47.7318177098045,31.0202629290117,-427.999999999991));
#36277=CARTESIAN_POINT('',(64.4405266043137,45.788778912222,-428.000078144656));
#36278=CARTESIAN_POINT('Origin',(0.00335440791743302,-11.16603510145,-427.999999999987));
#36279=CARTESIAN_POINT('',(56.7520934677589,53.4526994089804,-427.999999999993));
#36280=CARTESIAN_POINT('Origin',(0.00335440791743302,-11.16603510145,-427.999999999986));
#36281=CARTESIAN_POINT('',(56.7520925748523,53.4526983922443,-428.00007752232));
#36282=CARTESIAN_POINT('Origin',(35.1083877883366,28.8074139931111,-427.99999999999));
#36283=CARTESIAN_POINT('',(41.9923368054846,60.8737188148991,-427.999999331678));
#36284=CARTESIAN_POINT('Origin',(35.1083877883366,28.8074139931111,-427.99999999999));
#36285=CARTESIAN_POINT('Ctrl Pts',(41.9923369765522,60.8737187517663,-427.999999331209));
#36286=CARTESIAN_POINT('Ctrl Pts',(41.9758064463718,60.7967417673027,-432.332897601345));
#36287=CARTESIAN_POINT('Ctrl Pts',(41.9599261581031,60.7227955022272,-436.665849967173));
#36288=CARTESIAN_POINT('Ctrl Pts',(41.9454903641296,60.6521460670534,-440.99653250072));
#36289=CARTESIAN_POINT('Origin',(-0.0017653923509997,-134.670997806537,
-427.999999999971));
#36290=CARTESIAN_POINT('',(-41.9939391803561,60.8709610296021,-427.999999999994));
#36291=CARTESIAN_POINT('',(-41.9939390098067,60.870960235417,-428.000046536129));
#36292=CARTESIAN_POINT('Origin',(-0.0017653923509997,-134.670997806537,
-427.999999999972));
#36293=CARTESIAN_POINT('Origin',(-35.107222536544,28.8020791165365,-427.999999999989));
#36294=CARTESIAN_POINT('',(-56.7511891313755,53.4471346719238,-427.999999999992));
#36295=CARTESIAN_POINT('Origin',(-35.107222536544,28.8020791165365,-427.999999999989));
#36296=CARTESIAN_POINT('',(-56.7511885953632,53.4471340615896,-428.000046536128));
#36297=CARTESIAN_POINT('Origin',(-0.00176539236174112,-11.1709978065374,
-427.999999999985));
#36298=CARTESIAN_POINT('',(-64.435714908143,45.7874632814507,-427.999999999991));
#36299=CARTESIAN_POINT('Origin',(-0.00176539236174112,-11.1709978065374,
-427.999999999985));
#36300=CARTESIAN_POINT('',(-64.435714908143,45.7874632814507,-427.999999999991));
#36301=CARTESIAN_POINT('Origin',(-47.7278415015221,31.0180014613125,-427.99999999999));
#36302=CARTESIAN_POINT('',(-70.004366803487,32.0409661230246,-427.999999999987));
#36303=CARTESIAN_POINT('Origin',(-47.7278415015221,31.0180014613125,-427.99999999999));
#36304=CARTESIAN_POINT('',(-70.0043677413975,32.0409661660946,-427.999946210498));
#36305=CARTESIAN_POINT('Origin',(871.003976208289,-11.1712614676237,-427.99999999999));
#36306=CARTESIAN_POINT('Origin',(871.003976208289,-11.1712614676237,-427.99999999999));
#36307=CARTESIAN_POINT('Origin',(-25.500000000006,70.3310000000027,-303.499999999994));
#36308=CARTESIAN_POINT('',(47.9999999999939,71.3310000000091,-303.499999999995));
#36309=CARTESIAN_POINT('',(47.999999999994,70.3310000000091,-303.499999999994));
#36310=CARTESIAN_POINT('',(-51.0000000000061,71.331,-303.499999999995));
#36311=CARTESIAN_POINT('',(-51.000000000006,70.331,-303.499999999994));
#36312=CARTESIAN_POINT('',(-55.0000000000061,71.331,-303.499999999995));
#36313=CARTESIAN_POINT('Origin',(51.999999999994,70.3310000000035,-355.499999999994));
#36314=CARTESIAN_POINT('',(51.9999999999939,71.330999999998,-403.499999999995));
#36315=CARTESIAN_POINT('',(51.999999999994,70.330999999998,-403.499999999995));
#36316=CARTESIAN_POINT('',(51.9999999999939,71.331000000009,-307.499999999995));
#36317=CARTESIAN_POINT('',(51.999999999994,70.331000000009,-307.499999999994));
#36318=CARTESIAN_POINT('',(51.9999999999939,71.3309999999976,-407.499999999995));
#36319=CARTESIAN_POINT('Origin',(47.999999999994,70.3310000000087,-307.499999999994));
#36320=CARTESIAN_POINT('',(50.6457513110586,70.3310000000093,-304.499999999994));
#36321=CARTESIAN_POINT('Ctrl Pts',(50.6457513110591,70.3310000000092,-304.499999999995));
#36322=CARTESIAN_POINT('Ctrl Pts',(50.3169215545075,70.3310000000094,-304.20999941349));
#36323=CARTESIAN_POINT('Ctrl Pts',(49.8828383607448,70.4697262929124,-303.947060144719));
#36324=CARTESIAN_POINT('Ctrl Pts',(49.0403497074305,70.8111780179431,-303.605608419688));
#36325=CARTESIAN_POINT('Ctrl Pts',(48.4763938626813,71.0928030686654,-303.499999999995));
#36326=CARTESIAN_POINT('Ctrl Pts',(47.9999999999939,71.3310000000091,-303.499999999995));
#36327=CARTESIAN_POINT('',(50.9999999999939,70.3310000000092,-304.85424868893));
#36328=CARTESIAN_POINT('Origin',(47.999999999994,70.3310000000087,-307.499999999994));
#36329=CARTESIAN_POINT('Ctrl Pts',(51.9999999999939,71.331000000009,-307.499999999995));
#36330=CARTESIAN_POINT('Ctrl Pts',(51.9999999999939,71.0928030686655,-307.023606137307));
#36331=CARTESIAN_POINT('Ctrl Pts',(51.8943915803007,70.8111780179428,-306.459650292559));
#36332=CARTESIAN_POINT('Ctrl Pts',(51.5529398552703,70.4697262929124,-305.617161639245));
#36333=CARTESIAN_POINT('Ctrl Pts',(51.2900005864986,70.3310000000092,-305.183078445482));
#36334=CARTESIAN_POINT('Ctrl Pts',(50.999999999994,70.3310000000092,-304.85424868893));
#36335=CARTESIAN_POINT('Origin',(-1.50000000000603,70.3309999999929,-407.499999999995));
#36336=CARTESIAN_POINT('',(-51.0000000000061,71.3309999999886,-407.499999999995));
#36337=CARTESIAN_POINT('',(-51.000000000006,70.3309999999886,-407.499999999995));
#36338=CARTESIAN_POINT('',(47.9999999999939,71.3309999999972,-407.499999999995));
#36339=CARTESIAN_POINT('',(47.999999999994,70.3309999999972,-407.499999999995));
#36340=CARTESIAN_POINT('',(-55.0000000000061,71.3309999999882,-407.499999999995));
#36341=CARTESIAN_POINT('Origin',(47.999999999994,70.3309999999976,-403.499999999995));
#36342=CARTESIAN_POINT('',(50.9999999999939,70.3309999999976,-406.145751311059));
#36343=CARTESIAN_POINT('Ctrl Pts',(50.999999999994,70.3309999999976,-406.145751311059));
#36344=CARTESIAN_POINT('Ctrl Pts',(51.2900005864986,70.3309999999975,-405.816921554508));
#36345=CARTESIAN_POINT('Ctrl Pts',(51.5529398552703,70.4697262929009,-405.382838360744));
#36346=CARTESIAN_POINT('Ctrl Pts',(51.8943915803007,70.8111780179315,-404.54034970743));
#36347=CARTESIAN_POINT('Ctrl Pts',(51.9999999999939,71.0928030686541,-403.976393862682));
#36348=CARTESIAN_POINT('Ctrl Pts',(51.9999999999939,71.3309999999978,-403.499999999995));
#36349=CARTESIAN_POINT('',(50.6457513110586,70.3309999999976,-406.499999999995));
#36350=CARTESIAN_POINT('Origin',(47.999999999994,70.3309999999976,-403.499999999995));
#36351=CARTESIAN_POINT('Ctrl Pts',(47.9999999999939,71.3309999999972,-407.499999999995));
#36352=CARTESIAN_POINT('Ctrl Pts',(48.4763938626809,71.0928030686538,-407.499999999995));
#36353=CARTESIAN_POINT('Ctrl Pts',(49.0403497074289,70.8111780179308,-407.394391580302));
#36354=CARTESIAN_POINT('Ctrl Pts',(49.8828383607432,70.4697262929006,-407.052939855271));
#36355=CARTESIAN_POINT('Ctrl Pts',(50.3169215545064,70.3309999999975,-406.790000586499));
#36356=CARTESIAN_POINT('Ctrl Pts',(50.6457513110582,70.3309999999975,-406.499999999995));
#36357=CARTESIAN_POINT('Origin',(-51.000000000006,70.330999999989,-403.499999999995));
#36358=CARTESIAN_POINT('',(-53.6457513110706,70.3309999999884,-406.499999999995));
#36359=CARTESIAN_POINT('Ctrl Pts',(-53.6457513110702,70.3309999999884,-406.499999999995));
#36360=CARTESIAN_POINT('Ctrl Pts',(-53.271654714955,70.3309999999883,-406.82992218654));
#36361=CARTESIAN_POINT('Ctrl Pts',(-52.8397473959416,70.480582189106,-407.085008016199));
#36362=CARTESIAN_POINT('Ctrl Pts',(-51.9262909192953,70.8660628162156,-407.421591216636));
#36363=CARTESIAN_POINT('Ctrl Pts',(-51.4461362235074,71.1079318882378,-407.499999999995));
#36364=CARTESIAN_POINT('Ctrl Pts',(-51.0000000000061,71.3309999999885,-407.499999999995));
#36365=CARTESIAN_POINT('',(-54.0000000000059,70.3309999999884,-406.145751311059));
#36366=CARTESIAN_POINT('Origin',(-51.000000000006,70.330999999989,-403.499999999995));
#36367=CARTESIAN_POINT('',(-55.0000000000061,71.3309999999887,-403.499999999995));
#36368=CARTESIAN_POINT('Ctrl Pts',(-55.0000000000061,71.3309999999885,-403.499999999995));
#36369=CARTESIAN_POINT('Ctrl Pts',(-55.000000000006,71.092803068645,-403.976393862682));
#36370=CARTESIAN_POINT('Ctrl Pts',(-54.8943915803128,70.8111780179222,-404.54034970743));
#36371=CARTESIAN_POINT('Ctrl Pts',(-54.5529398552823,70.4697262928917,-405.382838360744));
#36372=CARTESIAN_POINT('Ctrl Pts',(-54.2900005865106,70.3309999999885,-405.816921554507));
#36373=CARTESIAN_POINT('Ctrl Pts',(-54.000000000006,70.3309999999885,-406.145751311059));
#36374=CARTESIAN_POINT('',(-55.000000000006,70.3309999999887,-403.499999999995));
#36375=CARTESIAN_POINT('Origin',(-51.000000000006,70.331,-307.499999999994));
#36376=CARTESIAN_POINT('',(-55.0000000000061,71.331,-307.499999999995));
#36377=CARTESIAN_POINT('',(-55.000000000006,70.331,-307.499999999994));
#36378=CARTESIAN_POINT('',(-54.0000000000059,70.331,-304.85424868893));
#36379=CARTESIAN_POINT('Ctrl Pts',(-54.000000000006,70.3310000000001,-304.85424868893));
#36380=CARTESIAN_POINT('Ctrl Pts',(-54.2900005865106,70.3310000000001,-305.183078445482));
#36381=CARTESIAN_POINT('Ctrl Pts',(-54.5529398552823,70.4697262929032,-305.617161639245));
#36382=CARTESIAN_POINT('Ctrl Pts',(-54.8943915803128,70.8111780179335,-306.459650292559));
#36383=CARTESIAN_POINT('Ctrl Pts',(-55.0000000000061,71.0928030686562,-307.023606137307));
#36384=CARTESIAN_POINT('Ctrl Pts',(-55.0000000000061,71.3309999999997,-307.499999999995));
#36385=CARTESIAN_POINT('',(-53.6457513110706,70.331,-304.499999999994));
#36386=CARTESIAN_POINT('Origin',(-51.000000000006,70.331,-307.499999999994));
#36387=CARTESIAN_POINT('Ctrl Pts',(-51.0000000000063,71.3310000000004,-303.499999999995));
#36388=CARTESIAN_POINT('Ctrl Pts',(-51.4461362235077,71.1079318882496,-303.499999999995));
#36389=CARTESIAN_POINT('Ctrl Pts',(-51.9262909192962,70.8660628162283,-303.578408783354));
#36390=CARTESIAN_POINT('Ctrl Pts',(-52.8397473959424,70.480582189118,-303.91499198379));
#36391=CARTESIAN_POINT('Ctrl Pts',(-53.2716547149558,70.3310000000002,-304.170077813449));
#36392=CARTESIAN_POINT('Ctrl Pts',(-53.6457513110711,70.3310000000001,-304.499999999995));
#36393=CARTESIAN_POINT('Origin',(-55.000000000006,70.3309999999942,-355.499999999994));
#36394=CARTESIAN_POINT('',(-55.0000000000061,71.3309999999882,-407.499999999995));
#36395=CARTESIAN_POINT('Ctrl Pts',(-71.7242220719942,-61.2914501133864,
-419.974938351021));
#36396=CARTESIAN_POINT('Ctrl Pts',(-71.723675161943,-61.2913712681343,-419.984638846289));
#36397=CARTESIAN_POINT('Ctrl Pts',(-71.2717722995097,-61.2262227212994,
-427.999999999979));
#36398=CARTESIAN_POINT('Ctrl Pts',(-71.2712259684214,-61.2261439595135,
-428.009690226232));
#36399=CARTESIAN_POINT('Ctrl Pts',(-71.7242858769396,-61.2947293352783,
-419.974938351021));
#36400=CARTESIAN_POINT('Ctrl Pts',(-71.7237373707235,-61.2946510609304,
-419.984638846289));
#36401=CARTESIAN_POINT('Ctrl Pts',(-71.2705156232134,-61.2299742429629,
-427.999999999979));
#36402=CARTESIAN_POINT('Ctrl Pts',(-71.26996769765,-61.2298960514769,-428.009690226232));
#36403=CARTESIAN_POINT('Ctrl Pts',(-71.724349681885,-61.2980085571703,-419.974938351021));
#36404=CARTESIAN_POINT('Ctrl Pts',(-71.723799579504,-61.2979308537266,-419.984638846289));
#36405=CARTESIAN_POINT('Ctrl Pts',(-71.2692589469172,-61.2337257646263,
-427.999999999979));
#36406=CARTESIAN_POINT('Ctrl Pts',(-71.2687094268786,-61.2336481434402,
-428.009690226232));
#36407=CARTESIAN_POINT('Ctrl Pts',(-71.7244134868304,-61.3012877790621,
-419.974938351021));
#36408=CARTESIAN_POINT('Ctrl Pts',(-71.7238617882844,-61.3012106465228,
-419.984638846289));
#36409=CARTESIAN_POINT('Ctrl Pts',(-71.2680022706209,-61.2374772862898,
-427.999999999979));
#36410=CARTESIAN_POINT('Ctrl Pts',(-71.267451156107,-61.2374002354035,-428.009690226232));
#36411=CARTESIAN_POINT('Ctrl Pts',(-71.7523909953645,-62.7391772385893,
-419.974938351021));
#36412=CARTESIAN_POINT('Ctrl Pts',(-71.7511394025092,-62.739350438968,-419.984638846289));
#36413=CARTESIAN_POINT('Ctrl Pts',(-70.7169686230121,-62.8824630892737,
-427.999999999979));
#36414=CARTESIAN_POINT('Ctrl Pts',(-70.715718355102,-62.8826361063013,-428.009690226232));
#36415=CARTESIAN_POINT('Ctrl Pts',(-71.7706749200703,-64.1748827234151,
-419.97493835102));
#36416=CARTESIAN_POINT('Ctrl Pts',(-71.7685254439165,-64.175261649583,-419.984638846288));
#36417=CARTESIAN_POINT('Ctrl Pts',(-69.9924483273783,-64.4883621667485,
-427.999999999978));
#36418=CARTESIAN_POINT('Ctrl Pts',(-69.9903011266753,-64.4887406917823,
-428.009690226232));
#36419=CARTESIAN_POINT('Ctrl Pts',(-71.7897768306913,-67.0361903512381,
-419.97493835102));
#36420=CARTESIAN_POINT('Ctrl Pts',(-71.7854748505741,-67.0367743707917,
-419.984638846288));
#36421=CARTESIAN_POINT('Ctrl Pts',(-68.2308187876847,-67.5193402102946,
-427.999999999978));
#36422=CARTESIAN_POINT('Ctrl Pts',(-68.2265213616744,-67.5199236116008,
-428.009690226232));
#36423=CARTESIAN_POINT('Ctrl Pts',(-71.7906156729946,-68.4617566097018,
-419.974938351019));
#36424=CARTESIAN_POINT('Ctrl Pts',(-71.7850594981988,-68.4623392639196,
-419.984638846288));
#36425=CARTESIAN_POINT('Ctrl Pts',(-67.1940828116454,-68.9437769487302,
-427.999999999977));
#36426=CARTESIAN_POINT('Ctrl Pts',(-67.188532518656,-68.9443589861462,-428.009690226231));
#36427=CARTESIAN_POINT('Ctrl Pts',(-71.7847586494582,-69.8799811589918,
-419.974938351019));
#36428=CARTESIAN_POINT('Ctrl Pts',(-71.7778115186237,-69.8804124953274,
-419.984638846288));
#36429=CARTESIAN_POINT('Ctrl Pts',(-66.0375105252458,-70.2368186801329,
-427.999999999977));
#36430=CARTESIAN_POINT('Ctrl Pts',(-66.0305707486938,-70.2372495598528,
-428.009690226231));
#36431=CARTESIAN_POINT('Ctrl Pts',(-71.7847466560944,-69.8828852420776,
-419.974938351019));
#36432=CARTESIAN_POINT('Ctrl Pts',(-71.7777966770143,-69.8833162685612,
-419.984638846288));
#36433=CARTESIAN_POINT('Ctrl Pts',(-66.0351422246716,-70.239466427715,-427.999999999977));
#36434=CARTESIAN_POINT('Ctrl Pts',(-66.0281996028891,-70.239896997911,-428.009690226231));
#36435=CARTESIAN_POINT('Ctrl Pts',(-71.7847346627306,-69.8857893251633,
-419.974938351019));
#36436=CARTESIAN_POINT('Ctrl Pts',(-71.7777818354048,-69.8862200417949,
-419.984638846288));
#36437=CARTESIAN_POINT('Ctrl Pts',(-66.0327739240975,-70.2421141752972,
-427.999999999977));
#36438=CARTESIAN_POINT('Ctrl Pts',(-66.0258284570844,-70.2425444359691,
-428.009690226231));
#36439=CARTESIAN_POINT('Ctrl Pts',(-71.7847226693668,-69.8886934082491,
-419.974938351019));
#36440=CARTESIAN_POINT('Ctrl Pts',(-71.7777669937953,-69.8891238150288,
-419.984638846288));
#36441=CARTESIAN_POINT('Ctrl Pts',(-66.0304056235233,-70.2447619228793,
-427.999999999977));
#36442=CARTESIAN_POINT('Ctrl Pts',(-66.0234573112798,-70.2451918740273,
-428.009690226231));
#36443=CARTESIAN_POINT('',(-66.0375105251866,-70.2368186801118,-427.999999999978));
#36444=CARTESIAN_POINT('',(-71.2680022706209,-61.2374772862897,-427.999999999979));
#36445=CARTESIAN_POINT('Ctrl Pts',(-66.0375105251866,-70.2368186801118,
-427.999999999978));
#36446=CARTESIAN_POINT('Ctrl Pts',(-67.1940828116442,-68.9437769487396,
-427.999999999967));
#36447=CARTESIAN_POINT('Ctrl Pts',(-68.2308187876832,-67.5193402103046,
-427.999999999967));
#36448=CARTESIAN_POINT('Ctrl Pts',(-69.9924483273808,-64.4883621667479,
-427.999999999967));
#36449=CARTESIAN_POINT('Ctrl Pts',(-70.7169686230136,-62.8824630892733,
-427.999999999968));
#36450=CARTESIAN_POINT('Ctrl Pts',(-71.2680022706209,-61.2374772862897,
-427.999999999979));
#36451=CARTESIAN_POINT('',(-71.6057458572746,-69.8910957793807,-420.224899491137));
#36452=CARTESIAN_POINT('',(-68.8215314165109,-70.063963238333,-424.112584875117));
#36453=CARTESIAN_POINT('',(-71.7785821060117,-69.7241904101603,-419.984638846415));
#36454=CARTESIAN_POINT('Origin',(-64.4008420418883,-77.3577815801559,-409.614647544567));
#36455=CARTESIAN_POINT('Ctrl Pts',(-71.268002270621,-61.2374772862896,-427.999999999978));
#36456=CARTESIAN_POINT('Ctrl Pts',(-71.2899303949503,-61.3466114274369,
-427.017655373544));
#36457=CARTESIAN_POINT('Ctrl Pts',(-71.3115444253862,-61.4774240219384,
-426.107461484164));
#36458=CARTESIAN_POINT('Ctrl Pts',(-71.3561812057394,-61.8206184542583,
-424.410282741723));
#36459=CARTESIAN_POINT('Ctrl Pts',(-71.3784339270585,-62.0406036470746,
-423.68637123802));
#36460=CARTESIAN_POINT('Ctrl Pts',(-71.4224149843577,-62.5795974842737,
-422.516016605151));
#36461=CARTESIAN_POINT('Ctrl Pts',(-71.4446474358491,-62.9048724301656,
-422.056379398897));
#36462=CARTESIAN_POINT('Ctrl Pts',(-71.4929560658814,-63.7151444243507,
-421.316245633231));
#36463=CARTESIAN_POINT('Ctrl Pts',(-71.5196071135653,-64.2098545996343,
-421.027118835742));
#36464=CARTESIAN_POINT('Ctrl Pts',(-71.605083940526,-65.9138105320977,-420.392921361503));
#36465=CARTESIAN_POINT('Ctrl Pts',(-71.6736227710617,-67.391175606321,-420.161937548972));
#36466=CARTESIAN_POINT('Ctrl Pts',(-71.7697681700019,-69.5279869464756,
-419.998805056281));
#36467=CARTESIAN_POINT('Ctrl Pts',(-71.774178781962,-69.6261206245261,-419.991593225368));
#36468=CARTESIAN_POINT('Ctrl Pts',(-71.7785821060559,-69.7241904101554,
-419.984638846373));
#36469=CARTESIAN_POINT('Ctrl Pts',(-71.6135253144154,-69.8855065275808,
-420.221597501086));
#36470=CARTESIAN_POINT('Ctrl Pts',(-71.6111594298038,-69.8856543483064,
-420.224899490927));
#36471=CARTESIAN_POINT('Ctrl Pts',(-66.0402789827285,-70.2337235592324,
-427.999999999977));
#36472=CARTESIAN_POINT('Ctrl Pts',(-66.0377194565801,-70.2338834787021,
-428.003572249148));
#36473=CARTESIAN_POINT('Ctrl Pts',(-71.6117204158214,-69.887320670077,-420.221597501086));
#36474=CARTESIAN_POINT('Ctrl Pts',(-71.6093549056591,-69.887468158653,-420.224899490927));
#36475=CARTESIAN_POINT('Ctrl Pts',(-66.0393561635675,-70.2347552661992,
-427.999999999977));
#36476=CARTESIAN_POINT('Ctrl Pts',(-66.0367970425162,-70.2349148263336,
-428.003572249148));
#36477=CARTESIAN_POINT('Ctrl Pts',(-71.6099155172274,-69.8891348125733,
-420.221597501086));
#36478=CARTESIAN_POINT('Ctrl Pts',(-71.6075503815144,-69.8892819689994,
-420.224899490927));
#36479=CARTESIAN_POINT('Ctrl Pts',(-66.0384333444067,-70.235786973166,-427.999999999977));
#36480=CARTESIAN_POINT('Ctrl Pts',(-66.0358746284523,-70.2359461739651,
-428.003572249148));
#36481=CARTESIAN_POINT('Ctrl Pts',(-71.6081106186334,-69.8909489550694,
-420.221597501086));
#36482=CARTESIAN_POINT('Ctrl Pts',(-71.6057458573697,-69.8910957793458,
-420.224899490927));
#36483=CARTESIAN_POINT('Ctrl Pts',(-66.0375105252458,-70.2368186801329,
-427.999999999977));
#36484=CARTESIAN_POINT('Ctrl Pts',(-66.0349522143885,-70.2369775215966,
-428.003572249148));
#36485=CARTESIAN_POINT('Ctrl Pts',(-69.4660550218801,-72.0439752249162,
-420.221597501086));
#36486=CARTESIAN_POINT('Ctrl Pts',(-69.4641346574427,-72.0437278535533,
-420.224899490927));
#36487=CARTESIAN_POINT('Ctrl Pts',(-64.9423077504781,-71.4612496203996,
-427.999999999977));
#36488=CARTESIAN_POINT('Ctrl Pts',(-64.940230209178,-71.4609820023305,-428.003572249148));
#36489=CARTESIAN_POINT('Ctrl Pts',(-67.3210277409069,-74.1944878424358,
-420.221597501085));
#36490=CARTESIAN_POINT('Ctrl Pts',(-67.3195381750349,-74.1938347731011,
-420.224899490927));
#36491=CARTESIAN_POINT('Ctrl Pts',(-63.8121002593275,-72.6560711942995,
-427.999999999977));
#36492=CARTESIAN_POINT('Ctrl Pts',(-63.8104887763412,-72.6553646729287,
-428.003572249148));
#36493=CARTESIAN_POINT('Ctrl Pts',(-63.0254878424137,-78.4900277409281,
-420.221597501084));
#36494=CARTESIAN_POINT('Ctrl Pts',(-63.0248347730789,-78.4885381750561,
-420.224899490927));
#36495=CARTESIAN_POINT('Ctrl Pts',(-61.4870711942769,-74.9811002593497,
-427.999999999977));
#36496=CARTESIAN_POINT('Ctrl Pts',(-61.4863646729061,-74.9794887763634,
-428.003572249148));
#36497=CARTESIAN_POINT('Ctrl Pts',(-60.8749752248937,-80.6350550219009,
-420.221597501084));
#36498=CARTESIAN_POINT('Ctrl Pts',(-60.8747278535309,-80.6331346574634,
-420.224899490927));
#36499=CARTESIAN_POINT('Ctrl Pts',(-60.2922496203767,-76.1113077505,-427.999999999977));
#36500=CARTESIAN_POINT('Ctrl Pts',(-60.2919820023077,-76.1092302091999,
-428.003572249148));
#36501=CARTESIAN_POINT('Ctrl Pts',(-58.7219489550468,-82.7771106186537,
-420.221597501084));
#36502=CARTESIAN_POINT('Ctrl Pts',(-58.7220957793232,-82.7747458573899,
-420.224899490926));
#36503=CARTESIAN_POINT('Ctrl Pts',(-59.0678186801098,-77.2065105252675,
-427.999999999977));
#36504=CARTESIAN_POINT('Ctrl Pts',(-59.0679775215736,-77.2039522144101,
-428.003572249148));
#36505=CARTESIAN_POINT('Ctrl Pts',(-58.7201348125564,-82.7789155172418,
-420.221597501084));
#36506=CARTESIAN_POINT('Ctrl Pts',(-58.7202819689826,-82.7765503815288,
-420.224899490926));
#36507=CARTESIAN_POINT('Ctrl Pts',(-59.0667869731464,-77.2074333444253,
-427.999999999977));
#36508=CARTESIAN_POINT('Ctrl Pts',(-59.0669461739455,-77.2048746284709,
-428.003572249148));
#36509=CARTESIAN_POINT('Ctrl Pts',(-58.7183206700661,-82.78072041583,-420.221597501084));
#36510=CARTESIAN_POINT('Ctrl Pts',(-58.718468158642,-82.7783549056677,-420.224899490926));
#36511=CARTESIAN_POINT('Ctrl Pts',(-59.0657552661828,-77.2083561635832,
-427.999999999977));
#36512=CARTESIAN_POINT('Ctrl Pts',(-59.0659148263172,-77.2057970425319,
-428.003572249148));
#36513=CARTESIAN_POINT('Ctrl Pts',(-58.7165065275757,-82.7825253144182,
-420.221597501084));
#36514=CARTESIAN_POINT('Ctrl Pts',(-58.7166543483013,-82.7801594298066,
-420.224899490926));
#36515=CARTESIAN_POINT('Ctrl Pts',(-59.0647235592194,-77.2092789827411,
-427.999999999977));
#36516=CARTESIAN_POINT('Ctrl Pts',(-59.0648834786889,-77.2067194565927,
-428.003572249148));
#36517=CARTESIAN_POINT('',(-59.0678186801297,-77.2065105251389,-427.999999999977));
#36518=CARTESIAN_POINT('Origin',(-31.3096336212146,-42.4786335233977,-427.999999993621));
#36519=CARTESIAN_POINT('',(-58.722095779334,-82.7747458573179,-420.224899491172));
#36520=CARTESIAN_POINT('',(-58.8896152555255,-80.0766663721036,-423.992311952553));
#36521=CARTESIAN_POINT('Ctrl Pts',(-71.6057458572757,-69.8910957793828,
-420.224899491013));
#36522=CARTESIAN_POINT('Ctrl Pts',(-71.5787972094958,-69.918039166144,-420.225112615511));
#36523=CARTESIAN_POINT('Ctrl Pts',(-71.3433559394484,-70.1534350994587,
-420.226949212009));
#36524=CARTESIAN_POINT('Ctrl Pts',(-71.0675267617563,-70.4292133340037,
-420.229012925027));
#36525=CARTESIAN_POINT('Ctrl Pts',(-70.9330282538967,-70.5636877197912,
-420.229990113068));
#36526=CARTESIAN_POINT('Ctrl Pts',(-70.5296622518239,-70.9669835947287,
-420.232830971758));
#36527=CARTESIAN_POINT('Ctrl Pts',(-70.2608984858126,-71.2357035867425,
-420.23460426166));
#36528=CARTESIAN_POINT('Ctrl Pts',(-69.4547425198419,-72.0417375568549,
-420.239546328562));
#36529=CARTESIAN_POINT('Ctrl Pts',(-68.9182881782136,-72.5781231052261,
-420.242333151682));
#36530=CARTESIAN_POINT('Ctrl Pts',(-67.305913743286,-74.1903309310481,-420.249082506593));
#36531=CARTESIAN_POINT('Ctrl Pts',(-66.238637509614,-75.2575503716149,-420.25138320211));
#36532=CARTESIAN_POINT('Ctrl Pts',(-64.088541529322,-77.4076463522807,-420.251383186951));
#36533=CARTESIAN_POINT('Ctrl Pts',(-63.021323830494,-78.4749208443966,-420.249082484014));
#36534=CARTESIAN_POINT('Ctrl Pts',(-61.4091186736197,-80.0872926103647,
-420.242333129556));
#36535=CARTESIAN_POINT('Ctrl Pts',(-60.8727340074292,-80.6237460697621,
-420.239546308457));
#36536=CARTESIAN_POINT('Ctrl Pts',(-60.0667013675136,-81.429900705396,-420.234604247222));
#36537=CARTESIAN_POINT('Ctrl Pts',(-59.7979818185861,-81.6986640282635,
-420.232830959641));
#36538=CARTESIAN_POINT('Ctrl Pts',(-59.3946866091394,-82.1020293647443,
-420.229990105046));
#36539=CARTESIAN_POINT('Ctrl Pts',(-59.2602124452137,-82.2365276507058,
-420.229012918471));
#36540=CARTESIAN_POINT('Ctrl Pts',(-58.9844213336794,-82.5123697077706,
-420.226949108894));
#36541=CARTESIAN_POINT('Ctrl Pts',(-58.7490049828989,-82.7478313994131,
-420.225112345118));
#36542=CARTESIAN_POINT('Ctrl Pts',(-58.7220957793367,-82.7747458573193,
-420.224899491011));
#36543=CARTESIAN_POINT('Ctrl Pts',(-58.7197046369747,-82.9535412049402,
-419.975191424209));
#36544=CARTESIAN_POINT('Ctrl Pts',(-58.7201238150062,-82.9467669938159,
-419.984638846285));
#36545=CARTESIAN_POINT('Ctrl Pts',(-59.0757619228566,-77.1994056235447,
-427.999999999977));
#36546=CARTESIAN_POINT('Ctrl Pts',(-59.0761804379555,-77.1926421258772,
-428.009432480898));
#36547=CARTESIAN_POINT('Ctrl Pts',(-58.7168005619725,-82.953553272611,-419.975191424209));
#36548=CARTESIAN_POINT('Ctrl Pts',(-58.7172200417724,-82.9467818354254,
-419.984638846285));
#36549=CARTESIAN_POINT('Ctrl Pts',(-59.0731141752743,-77.201773924119,-427.999999999977));
#36550=CARTESIAN_POINT('Ctrl Pts',(-59.0735329916644,-77.1950131960031,
-428.009432480898));
#36551=CARTESIAN_POINT('Ctrl Pts',(-58.7138964869703,-82.9535653402818,
-419.975191424209));
#36552=CARTESIAN_POINT('Ctrl Pts',(-58.7143162685385,-82.9467966770348,
-419.984638846285));
#36553=CARTESIAN_POINT('Ctrl Pts',(-59.070466427692,-77.2041422246933,-427.999999999977));
#36554=CARTESIAN_POINT('Ctrl Pts',(-59.0708855453734,-77.197384266129,-428.009432480898));
#36555=CARTESIAN_POINT('Ctrl Pts',(-58.710992411968,-82.9535774079526,-419.975191424209));
#36556=CARTESIAN_POINT('Ctrl Pts',(-58.7114124953047,-82.9468115186443,
-419.984638846285));
#36557=CARTESIAN_POINT('Ctrl Pts',(-59.0678186801098,-77.2065105252675,
-427.999999999977));
#36558=CARTESIAN_POINT('Ctrl Pts',(-59.0682380990822,-77.199755336255,-428.009432480898));
#36559=CARTESIAN_POINT('Ctrl Pts',(-57.2927718103627,-82.9594707197063,
-419.975191424209));
#36560=CARTESIAN_POINT('Ctrl Pts',(-57.2933392638967,-82.9540594982192,
-419.984638846285));
#36561=CARTESIAN_POINT('Ctrl Pts',(-57.7747769487071,-78.3630828116667,
-427.999999999977));
#36562=CARTESIAN_POINT('Ctrl Pts',(-57.7753435048097,-78.3576801480598,
-428.009432480898));
#36563=CARTESIAN_POINT('Ctrl Pts',(-55.8672055875188,-82.958664597696,-419.975191424209));
#36564=CARTESIAN_POINT('Ctrl Pts',(-55.8677743707687,-82.9544748505942,
-419.984638846285));
#36565=CARTESIAN_POINT('Ctrl Pts',(-56.3503402102711,-79.3998187877058,
-427.999999999977));
#36566=CARTESIAN_POINT('Ctrl Pts',(-56.3509080939867,-79.395635666715,-428.009432480898));
#36567=CARTESIAN_POINT('Ctrl Pts',(-53.0058926090782,-82.9396188430779,
-419.975191424209));
#36568=CARTESIAN_POINT('Ctrl Pts',(-53.0062616495595,-82.937525443936,-419.984638846285));
#36569=CARTESIAN_POINT('Ctrl Pts',(-53.3193621667245,-81.1614483273987,
-427.999999999976));
#36570=CARTESIAN_POINT('Ctrl Pts',(-53.3197306235661,-81.1593582389807,
-428.009432480897));
#36571=CARTESIAN_POINT('Ctrl Pts',(-51.5701817571364,-82.9213583429688,
-419.975191424209));
#36572=CARTESIAN_POINT('Ctrl Pts',(-51.5703504389445,-82.9201394025285,
-419.984638846286));
#36573=CARTESIAN_POINT('Ctrl Pts',(-51.7134630892495,-81.8859686230323,
-427.999999999976));
#36574=CARTESIAN_POINT('Ctrl Pts',(-51.7136315042863,-81.8847516103539,
-428.009432480897));
#36575=CARTESIAN_POINT('Ctrl Pts',(-50.1322857667517,-82.8933990937584,
-419.975191424209));
#36576=CARTESIAN_POINT('Ctrl Pts',(-50.1322106464991,-82.8928617883035,
-419.984638846286));
#36577=CARTESIAN_POINT('Ctrl Pts',(-50.0684772862654,-82.4370022706408,
-427.999999999976));
#36578=CARTESIAN_POINT('Ctrl Pts',(-50.068402284816,-82.4364658149378,-428.009432480897));
#36579=CARTESIAN_POINT('Ctrl Pts',(-50.1290939798984,-82.89333703088,-419.975191424209));
#36580=CARTESIAN_POINT('Ctrl Pts',(-50.1290183184633,-82.8928012384925,
-419.984638846286));
#36581=CARTESIAN_POINT('Ctrl Pts',(-50.0648258093193,-82.4382254341825,
-427.999999999976));
#36582=CARTESIAN_POINT('Ctrl Pts',(-50.0647502675432,-82.4376904891539,
-428.009432480897));
#36583=CARTESIAN_POINT('Ctrl Pts',(-50.1259021930451,-82.8932749680016,
-419.975191424209));
#36584=CARTESIAN_POINT('Ctrl Pts',(-50.1258259904275,-82.8927406886815,
-419.984638846286));
#36585=CARTESIAN_POINT('Ctrl Pts',(-50.0611743323731,-82.4394485977242,
-427.999999999976));
#36586=CARTESIAN_POINT('Ctrl Pts',(-50.0610982502703,-82.4389151633701,
-428.009432480897));
#36587=CARTESIAN_POINT('Ctrl Pts',(-50.1227104061918,-82.8932129051231,
-419.975191424209));
#36588=CARTESIAN_POINT('Ctrl Pts',(-50.1226336623915,-82.8926801388705,
-419.984638846286));
#36589=CARTESIAN_POINT('Ctrl Pts',(-50.057522855427,-82.4406717612658,-427.999999999976));
#36590=CARTESIAN_POINT('Ctrl Pts',(-50.0574462329975,-82.4401398375863,
-428.009432480897));
#36591=CARTESIAN_POINT('',(-50.0684772862639,-82.4370022706413,-427.999999999976));
#36592=CARTESIAN_POINT('Ctrl Pts',(-50.0684772862639,-82.4370022706413,
-427.999999999976));
#36593=CARTESIAN_POINT('Ctrl Pts',(-51.7134630892489,-81.8859686230341,
-427.999999999963));
#36594=CARTESIAN_POINT('Ctrl Pts',(-53.3193621667236,-81.1614483274017,
-427.999999999963));
#36595=CARTESIAN_POINT('Ctrl Pts',(-56.3503402102723,-79.3998187877103,
-427.999999999964));
#36596=CARTESIAN_POINT('Ctrl Pts',(-57.7747769487082,-78.3630828116726,
-427.999999999964));
#36597=CARTESIAN_POINT('Ctrl Pts',(-59.0678186801297,-77.2065105251389,
-427.999999999977));
#36598=CARTESIAN_POINT('',(-58.5551904101346,-82.9475821060765,-419.98463884637));
#36599=CARTESIAN_POINT('Ctrl Pts',(-58.5551904101346,-82.9475821060766,
-419.98463884637));
#36600=CARTESIAN_POINT('Ctrl Pts',(-58.4188729154943,-82.9414614634676,
-419.994305468106));
#36601=CARTESIAN_POINT('Ctrl Pts',(-58.2823655888712,-82.9353237594846,
-420.004474223787));
#36602=CARTESIAN_POINT('Ctrl Pts',(-56.066191044342,-82.8355192518713,-420.178712470519));
#36603=CARTESIAN_POINT('Ctrl Pts',(-54.6525784405451,-82.769565172487,-420.421071349311));
#36604=CARTESIAN_POINT('Ctrl Pts',(-53.0155721288554,-82.6872714498112,
-421.040386425013));
#36605=CARTESIAN_POINT('Ctrl Pts',(-52.5265838564269,-82.6608599495699,
-421.330101387063));
#36606=CARTESIAN_POINT('Ctrl Pts',(-51.7205137979776,-82.6126582331124,
-422.074616347874));
#36607=CARTESIAN_POINT('Ctrl Pts',(-51.3955527915526,-82.5903403336599,
-422.539928724141));
#36608=CARTESIAN_POINT('Ctrl Pts',(-50.8567852682764,-82.5460626358379,
-423.727827254023));
#36609=CARTESIAN_POINT('Ctrl Pts',(-50.6369357056377,-82.5235929056932,
-424.464498286675));
#36610=CARTESIAN_POINT('Ctrl Pts',(-50.2838325468242,-82.4770364056074,
-426.246791579634));
#36611=CARTESIAN_POINT('Ctrl Pts',(-50.1582077546299,-82.4550316503171,
-427.192312850031));
#36612=CARTESIAN_POINT('Ctrl Pts',(-50.0684772862656,-82.4370022706407,
-427.999999999976));
#36613=CARTESIAN_POINT('Origin',(-66.1887815785501,-75.5698420254738,-409.614647535942));
#36614=CARTESIAN_POINT('Ctrl Pts',(58.7197056437309,-82.9535249352716,-419.975214114133));
#36615=CARTESIAN_POINT('Ctrl Pts',(58.7201238150205,-82.9467669938057,-419.984638846287));
#36616=CARTESIAN_POINT('Ctrl Pts',(59.0757619228695,-77.1994056235345,-427.999999999979));
#36617=CARTESIAN_POINT('Ctrl Pts',(59.0761795998615,-77.1926556702662,-428.009413591666));
#36618=CARTESIAN_POINT('Ctrl Pts',(58.7168015694534,-82.9535370096046,-419.975214114133));
#36619=CARTESIAN_POINT('Ctrl Pts',(58.7172200417867,-82.9467818354151,-419.984638846287));
#36620=CARTESIAN_POINT('Ctrl Pts',(59.0731141752874,-77.2017739241088,-427.999999999979));
#36621=CARTESIAN_POINT('Ctrl Pts',(59.073532152967,-77.1950267348458,-428.009413591666));
#36622=CARTESIAN_POINT('Ctrl Pts',(58.7138974951761,-82.9535490839376,-419.975214114133));
#36623=CARTESIAN_POINT('Ctrl Pts',(58.7143162685529,-82.9467966770246,-419.984638846287));
#36624=CARTESIAN_POINT('Ctrl Pts',(59.0704664277052,-77.204142224683,-427.999999999979));
#36625=CARTESIAN_POINT('Ctrl Pts',(59.0708847060726,-77.1973977994254,-428.009413591666));
#36626=CARTESIAN_POINT('Ctrl Pts',(58.7109934208987,-82.9535611582706,-419.975214114133));
#36627=CARTESIAN_POINT('Ctrl Pts',(58.7114124953191,-82.9468115186341,-419.984638846287));
#36628=CARTESIAN_POINT('Ctrl Pts',(59.067818680123,-77.2065105252572,-427.999999999979));
#36629=CARTESIAN_POINT('Ctrl Pts',(59.0682372591782,-77.1997688640051,-428.009413591664));
#36630=CARTESIAN_POINT('Ctrl Pts',(57.2927731732331,-82.9594577235373,-419.975214114133));
#36631=CARTESIAN_POINT('Ctrl Pts',(57.293339263911,-82.9540594982091,-419.984638846287));
#36632=CARTESIAN_POINT('Ctrl Pts',(57.7747769487204,-78.3630828116567,-427.999999999979));
#36633=CARTESIAN_POINT('Ctrl Pts',(57.775342370253,-78.3576909672791,-428.009413591664));
#36634=CARTESIAN_POINT('Ctrl Pts',(55.8672069535827,-82.9586545351486,-419.975214114133));
#36635=CARTESIAN_POINT('Ctrl Pts',(55.867774370783,-82.9544748505844,-419.984638846287));
#36636=CARTESIAN_POINT('Ctrl Pts',(56.3503402102845,-79.399818787696,-427.999999999979));
#36637=CARTESIAN_POINT('Ctrl Pts',(56.3509069567715,-79.3956440437112,-428.009413591664));
#36638=CARTESIAN_POINT('Ctrl Pts',(53.0058934954191,-82.939613815341,-419.975214114133));
#36639=CARTESIAN_POINT('Ctrl Pts',(53.0062616495739,-82.9375254439268,-419.984638846287));
#36640=CARTESIAN_POINT('Ctrl Pts',(53.3193621667384,-81.1614483273895,-427.999999999979));
#36641=CARTESIAN_POINT('Ctrl Pts',(53.3197298857181,-81.1593624245264,-428.009413591664));
#36642=CARTESIAN_POINT('Ctrl Pts',(51.5701821622747,-82.9213554154241,-419.975214114133));
#36643=CARTESIAN_POINT('Ctrl Pts',(51.5703504389588,-82.9201394025195,-419.984638846287));
#36644=CARTESIAN_POINT('Ctrl Pts',(51.7134630892636,-81.8859686230233,-427.999999999978));
#36645=CARTESIAN_POINT('Ctrl Pts',(51.7136311670369,-81.8847540475019,-428.009413591664));
#36646=CARTESIAN_POINT('Ctrl Pts',(50.1322855863494,-82.8933978033003,-419.975214114133));
#36647=CARTESIAN_POINT('Ctrl Pts',(50.1322106465135,-82.8928617882947,-419.984638846287));
#36648=CARTESIAN_POINT('Ctrl Pts',(50.0684772862794,-82.437002270632,-427.999999999978));
#36649=CARTESIAN_POINT('Ctrl Pts',(50.0684024350259,-82.4364668892208,-428.009413591664));
#36650=CARTESIAN_POINT('Ctrl Pts',(50.1290999320919,-82.8933358633196,-419.975214114133));
#36651=CARTESIAN_POINT('Ctrl Pts',(50.1290244534106,-82.8928013548467,-419.984638846287));
#36652=CARTESIAN_POINT('Ctrl Pts',(50.0648328266468,-82.4382230835297,-427.999999999978));
#36653=CARTESIAN_POINT('Ctrl Pts',(50.0647574371849,-82.4376892068704,-428.009413591664));
#36654=CARTESIAN_POINT('Ctrl Pts',(50.1259142778343,-82.893273923339,-419.975214114133));
#36655=CARTESIAN_POINT('Ctrl Pts',(50.1258382603078,-82.8927409213988,-419.984638846287));
#36656=CARTESIAN_POINT('Ctrl Pts',(50.0611883670142,-82.4394438964275,-427.999999999978));
#36657=CARTESIAN_POINT('Ctrl Pts',(50.061112439344,-82.4389115245201,-428.009413591664));
#36658=CARTESIAN_POINT('Ctrl Pts',(50.1227286235768,-82.8932119833583,-419.975214114133));
#36659=CARTESIAN_POINT('Ctrl Pts',(50.1226520672052,-82.8926804879508,-419.984638846287));
#36660=CARTESIAN_POINT('Ctrl Pts',(50.0575439073816,-82.4406647093253,-427.999999999978));
#36661=CARTESIAN_POINT('Ctrl Pts',(50.0574674415031,-82.4401338421698,-428.009413591664));
#36662=CARTESIAN_POINT('',(58.7220957793721,-82.7747458572873,-420.224899491043));
#36663=CARTESIAN_POINT('',(59.0678186800936,-77.2065105252676,-427.999999999979));
#36664=CARTESIAN_POINT('',(58.8949632383239,-79.9905314165215,-424.112584875118));
#36665=CARTESIAN_POINT('',(58.5551904101516,-82.947582106022,-419.984638846415));
#36666=CARTESIAN_POINT('Origin',(66.1887816381845,-75.569842237361,-409.61464764338));
#36667=CARTESIAN_POINT('',(50.0684772862795,-82.4370022706321,-427.999999999977));
#36668=CARTESIAN_POINT('Ctrl Pts',(50.0684772862793,-82.437002270632,-427.999999999977));
#36669=CARTESIAN_POINT('Ctrl Pts',(50.1776098648765,-82.4589300810008,-427.017669438463));
#36670=CARTESIAN_POINT('Ctrl Pts',(50.3084199515129,-82.4805437409056,-426.10749048955));
#36671=CARTESIAN_POINT('Ctrl Pts',(50.6516098353792,-82.5251802709515,-424.410314707175));
#36672=CARTESIAN_POINT('Ctrl Pts',(50.8715944931139,-82.5474330763281,-423.686397055261));
#36673=CARTESIAN_POINT('Ctrl Pts',(51.410590597809,-82.5914145260594,-422.516025627724));
#36674=CARTESIAN_POINT('Ctrl Pts',(51.7358697925533,-82.6136472976727,-422.056380716835));
#36675=CARTESIAN_POINT('Ctrl Pts',(52.5461423541371,-82.6619559233828,-421.316248616454));
#36676=CARTESIAN_POINT('Ctrl Pts',(53.0408434762955,-82.688606506298,-421.027125796862));
#36677=CARTESIAN_POINT('Ctrl Pts',(54.7447370654671,-82.7740803411882,-420.392943782119));
#36678=CARTESIAN_POINT('Ctrl Pts',(56.2220249700593,-82.8426158585167,-420.161956759134));
#36679=CARTESIAN_POINT('Ctrl Pts',(58.3588571103766,-82.9387623345377,-419.998814597882));
#36680=CARTESIAN_POINT('Ctrl Pts',(58.4570557771101,-82.9431758703299,-419.991597823863));
#36681=CARTESIAN_POINT('Ctrl Pts',(58.5551904101466,-82.9475821060663,-419.984638846372));
#36682=CARTESIAN_POINT('Ctrl Pts',(59.0678186800936,-77.2065105252676,-427.999999999979));
#36683=CARTESIAN_POINT('Ctrl Pts',(57.7747769487207,-78.3630828116585,-427.999999999975));
#36684=CARTESIAN_POINT('Ctrl Pts',(56.3503402102848,-79.3998187876973,-427.999999999975));
#36685=CARTESIAN_POINT('Ctrl Pts',(53.3193621667383,-81.1614483273903,-427.999999999975));
#36686=CARTESIAN_POINT('Ctrl Pts',(51.7134630892636,-81.8859686230238,-427.999999999974));
#36687=CARTESIAN_POINT('Ctrl Pts',(50.0684772862795,-82.4370022706321,-427.999999999977));
#36688=CARTESIAN_POINT('Ctrl Pts',(71.6135253144103,-69.8855065275854,-420.221597501088));
#36689=CARTESIAN_POINT('Ctrl Pts',(71.6111594297988,-69.885654348311,-420.224899490929));
#36690=CARTESIAN_POINT('Ctrl Pts',(66.0402789827317,-70.2337235592304,-427.99999999998));
#36691=CARTESIAN_POINT('Ctrl Pts',(66.0377194565832,-70.2338834787001,-428.00357224915));
#36692=CARTESIAN_POINT('Ctrl Pts',(71.611720415822,-69.8873206700759,-420.221597501088));
#36693=CARTESIAN_POINT('Ctrl Pts',(71.6093549056598,-69.8874681586518,-420.224899490929));
#36694=CARTESIAN_POINT('Ctrl Pts',(66.0393561635738,-70.2347552661941,-427.99999999998));
#36695=CARTESIAN_POINT('Ctrl Pts',(66.0367970425222,-70.2349148263284,-428.00357224915));
#36696=CARTESIAN_POINT('Ctrl Pts',(71.6099155172337,-69.8891348125665,-420.221597501088));
#36697=CARTESIAN_POINT('Ctrl Pts',(71.6075503815208,-69.8892819689926,-420.224899490929));
#36698=CARTESIAN_POINT('Ctrl Pts',(66.0384333444158,-70.2357869731577,-427.99999999998));
#36699=CARTESIAN_POINT('Ctrl Pts',(66.0358746284611,-70.2359461739567,-428.00357224915));
#36700=CARTESIAN_POINT('Ctrl Pts',(71.6081106186453,-69.8909489550569,-420.221597501088));
#36701=CARTESIAN_POINT('Ctrl Pts',(71.6057458573818,-69.8910957793334,-420.224899490929));
#36702=CARTESIAN_POINT('Ctrl Pts',(66.0375105252578,-70.2368186801213,-427.99999999998));
#36703=CARTESIAN_POINT('Ctrl Pts',(66.0349522144002,-70.236977521585,-428.00357224915));
#36704=CARTESIAN_POINT('Ctrl Pts',(69.4660550218924,-72.0439752249039,-420.221597501088));
#36705=CARTESIAN_POINT('Ctrl Pts',(69.4641346574551,-72.0437278535411,-420.224899490929));
#36706=CARTESIAN_POINT('Ctrl Pts',(64.9423077504902,-71.4612496203883,-427.99999999998));
#36707=CARTESIAN_POINT('Ctrl Pts',(64.94023020919,-71.460982002319,-428.00357224915));
#36708=CARTESIAN_POINT('Ctrl Pts',(67.3210277409196,-74.194487842424,-420.221597501087));
#36709=CARTESIAN_POINT('Ctrl Pts',(67.3195381750477,-74.1938347730893,-420.224899490929));
#36710=CARTESIAN_POINT('Ctrl Pts',(63.8121002593399,-72.6560711942883,-427.999999999979));
#36711=CARTESIAN_POINT('Ctrl Pts',(63.8104887763535,-72.6553646729174,-428.00357224915));
#36712=CARTESIAN_POINT('Ctrl Pts',(63.0254878424273,-78.4900277409171,-420.221597501087));
#36713=CARTESIAN_POINT('Ctrl Pts',(63.0248347730926,-78.4885381750452,-420.224899490929));
#36714=CARTESIAN_POINT('Ctrl Pts',(61.4870711942897,-74.9811002593389,-427.999999999979));
#36715=CARTESIAN_POINT('Ctrl Pts',(61.4863646729188,-74.9794887763524,-428.00357224915));
#36716=CARTESIAN_POINT('Ctrl Pts',(60.8749752249077,-80.6350550218902,-420.221597501087));
#36717=CARTESIAN_POINT('Ctrl Pts',(60.8747278535448,-80.6331346574529,-420.224899490929));
#36718=CARTESIAN_POINT('Ctrl Pts',(60.2922496203898,-76.1113077504894,-427.999999999979));
#36719=CARTESIAN_POINT('Ctrl Pts',(60.2919820023206,-76.1092302091891,-428.00357224915));
#36720=CARTESIAN_POINT('Ctrl Pts',(58.721948955061,-82.7771106186434,-420.221597501086));
#36721=CARTESIAN_POINT('Ctrl Pts',(58.7220957793374,-82.7747458573798,-420.224899490928));
#36722=CARTESIAN_POINT('Ctrl Pts',(59.067818680123,-77.2065105252572,-427.999999999979));
#36723=CARTESIAN_POINT('Ctrl Pts',(59.0679775215867,-77.2039522143996,-428.00357224915));
#36724=CARTESIAN_POINT('Ctrl Pts',(58.7201348125646,-82.7789155172375,-420.221597501086));
#36725=CARTESIAN_POINT('Ctrl Pts',(58.7202819689909,-82.7765503815246,-420.224899490928));
#36726=CARTESIAN_POINT('Ctrl Pts',(59.0667869731561,-77.2074333444181,-427.999999999979));
#36727=CARTESIAN_POINT('Ctrl Pts',(59.0669461739552,-77.2048746284635,-428.00357224915));
#36728=CARTESIAN_POINT('Ctrl Pts',(58.7183206700682,-82.7807204158317,-420.221597501086));
#36729=CARTESIAN_POINT('Ctrl Pts',(58.7184681586442,-82.7783549056695,-420.224899490928));
#36730=CARTESIAN_POINT('Ctrl Pts',(59.0657552661892,-77.2083561635791,-427.999999999979));
#36731=CARTESIAN_POINT('Ctrl Pts',(59.0659148263236,-77.2057970425275,-428.00357224915));
#36732=CARTESIAN_POINT('Ctrl Pts',(58.716506527572,-82.7825253144258,-420.221597501086));
#36733=CARTESIAN_POINT('Ctrl Pts',(58.7166543482976,-82.7801594298143,-420.224899490928));
#36734=CARTESIAN_POINT('Ctrl Pts',(59.0647235592222,-77.20927898274,-427.999999999977));
#36735=CARTESIAN_POINT('Ctrl Pts',(59.0648834786919,-77.2067194565913,-428.00357224915));
#36736=CARTESIAN_POINT('',(71.605745857323,-69.891095779332,-420.224899491139));
#36737=CARTESIAN_POINT('',(66.0375105251256,-70.2368186801723,-427.99999999998));
#36738=CARTESIAN_POINT('',(68.9076646990879,-70.0586153594102,-423.992314288627));
#36739=CARTESIAN_POINT('Ctrl Pts',(58.7220957793725,-82.7747458572875,-420.224899491013));
#36740=CARTESIAN_POINT('Ctrl Pts',(58.7490050273729,-82.7478313549345,-420.225112345472));
#36741=CARTESIAN_POINT('Ctrl Pts',(58.9844242521529,-82.5123667887596,-420.226949130836));
#36742=CARTESIAN_POINT('Ctrl Pts',(59.2602133340799,-82.2365267616816,-420.229012925029));
#36743=CARTESIAN_POINT('Ctrl Pts',(59.3946877198224,-82.1020282538672,-420.229990113069));
#36744=CARTESIAN_POINT('Ctrl Pts',(59.7979835946476,-81.6986622519067,-420.232830971759));
#36745=CARTESIAN_POINT('Ctrl Pts',(60.066703586697,-81.4298984858598,-420.234604261661));
#36746=CARTESIAN_POINT('Ctrl Pts',(60.8727375567166,-80.6237425199819,-420.239546328562));
#36747=CARTESIAN_POINT('Ctrl Pts',(61.4091231051532,-80.0872881782882,-420.242333151683));
#36748=CARTESIAN_POINT('Ctrl Pts',(63.0213309310981,-78.4749137432377,-420.249082506595));
#36749=CARTESIAN_POINT('Ctrl Pts',(64.0885503716301,-77.4076375096007,-420.251383202111));
#36750=CARTESIAN_POINT('Ctrl Pts',(66.2386463522281,-75.2575415293765,-420.251383186953));
#36751=CARTESIAN_POINT('Ctrl Pts',(67.3059208443083,-74.1903238305842,-420.249082484017));
#36752=CARTESIAN_POINT('Ctrl Pts',(68.918292610394,-72.5781186735924,-420.242333129559));
#36753=CARTESIAN_POINT('Ctrl Pts',(69.4547460698333,-72.0417340073601,-420.239546308459));
#36754=CARTESIAN_POINT('Ctrl Pts',(70.2609007054355,-71.2357013674762,-420.234604247225));
#36755=CARTESIAN_POINT('Ctrl Pts',(70.529664028348,-70.9669818185037,-420.232830959644));
#36756=CARTESIAN_POINT('Ctrl Pts',(70.9330293646617,-70.563686609224,-420.229990105049));
#36757=CARTESIAN_POINT('Ctrl Pts',(71.0675276505347,-70.4292124453869,-420.229012918476));
#36758=CARTESIAN_POINT('Ctrl Pts',(71.3433567842835,-70.1534342547818,-420.226949205589));
#36759=CARTESIAN_POINT('Ctrl Pts',(71.578797254063,-69.9180391215851,-420.225112615161));
#36760=CARTESIAN_POINT('Ctrl Pts',(71.605745857324,-69.891095779334,-420.224899491015));
#36761=CARTESIAN_POINT('Origin',(31.3096308343611,-42.4786310540604,-427.999999997311));
#36762=CARTESIAN_POINT('Ctrl Pts',(71.7242220720048,-61.2914501133736,-419.974938351023));
#36763=CARTESIAN_POINT('Ctrl Pts',(71.7236751619536,-61.2913712681216,-419.98463884629));
#36764=CARTESIAN_POINT('Ctrl Pts',(71.2717722995202,-61.2262227212868,-427.999999999981));
#36765=CARTESIAN_POINT('Ctrl Pts',(71.2712259684319,-61.2261439595009,-428.009690226235));
#36766=CARTESIAN_POINT('Ctrl Pts',(71.7242858769502,-61.2947293352656,-419.974938351023));
#36767=CARTESIAN_POINT('Ctrl Pts',(71.7237373707341,-61.2946510609178,-419.98463884629));
#36768=CARTESIAN_POINT('Ctrl Pts',(71.2705156232239,-61.2299742429503,-427.999999999981));
#36769=CARTESIAN_POINT('Ctrl Pts',(71.2699676976604,-61.2298960514643,-428.009690226235));
#36770=CARTESIAN_POINT('Ctrl Pts',(71.7243496818956,-61.2980085571576,-419.974938351023));
#36771=CARTESIAN_POINT('Ctrl Pts',(71.7237995795144,-61.2979308537141,-419.98463884629));
#36772=CARTESIAN_POINT('Ctrl Pts',(71.2692589469276,-61.2337257646139,-427.999999999981));
#36773=CARTESIAN_POINT('Ctrl Pts',(71.2687094268889,-61.2336481434277,-428.009690226235));
#36774=CARTESIAN_POINT('Ctrl Pts',(71.724413486841,-61.3012877790496,-419.974938351023));
#36775=CARTESIAN_POINT('Ctrl Pts',(71.723861788295,-61.3012106465104,-419.98463884629));
#36776=CARTESIAN_POINT('Ctrl Pts',(71.2680022706313,-61.2374772862774,-427.999999999981));
#36777=CARTESIAN_POINT('Ctrl Pts',(71.2674511561174,-61.2374002353911,-428.009690226235));
#36778=CARTESIAN_POINT('Ctrl Pts',(71.7523909953753,-62.7391772385768,-419.974938351023));
#36779=CARTESIAN_POINT('Ctrl Pts',(71.75113940252,-62.7393504389554,-419.98463884629));
#36780=CARTESIAN_POINT('Ctrl Pts',(70.7169686230227,-62.8824630892614,-427.999999999981));
#36781=CARTESIAN_POINT('Ctrl Pts',(70.7157183551126,-62.882636106289,-428.009690226235));
#36782=CARTESIAN_POINT('Ctrl Pts',(71.7706749200814,-64.1748827234026,-419.974938351022));
#36783=CARTESIAN_POINT('Ctrl Pts',(71.7685254439275,-64.1752616495704,-419.98463884629));
#36784=CARTESIAN_POINT('Ctrl Pts',(69.9924483273891,-64.4883621667363,-427.99999999998));
#36785=CARTESIAN_POINT('Ctrl Pts',(69.9903011266861,-64.4887406917701,-428.009690226234));
#36786=CARTESIAN_POINT('Ctrl Pts',(71.789776830703,-67.0361903512256,-419.974938351022));
#36787=CARTESIAN_POINT('Ctrl Pts',(71.7854748505856,-67.0367743707791,-419.984638846289));
#36788=CARTESIAN_POINT('Ctrl Pts',(68.2308187876961,-67.5193402102826,-427.99999999998));
#36789=CARTESIAN_POINT('Ctrl Pts',(68.2265213616857,-67.5199236115889,-428.009690226233));
#36790=CARTESIAN_POINT('Ctrl Pts',(71.7906156730065,-68.4617566096892,-419.974938351022));
#36791=CARTESIAN_POINT('Ctrl Pts',(71.7850594982106,-68.462339263907,-419.984638846289));
#36792=CARTESIAN_POINT('Ctrl Pts',(67.194082811657,-68.9437769487185,-427.99999999998));
#36793=CARTESIAN_POINT('Ctrl Pts',(67.1885325186674,-68.9443589861345,-428.009690226233));
#36794=CARTESIAN_POINT('Ctrl Pts',(71.7847586494703,-69.8799811589792,-419.974938351022));
#36795=CARTESIAN_POINT('Ctrl Pts',(71.7778115186357,-69.8804124953149,-419.984638846289));
#36796=CARTESIAN_POINT('Ctrl Pts',(66.0375105252578,-70.2368186801213,-427.99999999998));
#36797=CARTESIAN_POINT('Ctrl Pts',(66.0305707487055,-70.2372495598412,-428.009690226233));
#36798=CARTESIAN_POINT('Ctrl Pts',(71.7847466561065,-69.8828852420651,-419.974938351022));
#36799=CARTESIAN_POINT('Ctrl Pts',(71.7777966770263,-69.8833162685488,-419.984638846289));
#36800=CARTESIAN_POINT('Ctrl Pts',(66.0351422246835,-70.2394664277036,-427.99999999998));
#36801=CARTESIAN_POINT('Ctrl Pts',(66.0281996029007,-70.2398969978995,-428.009690226233));
#36802=CARTESIAN_POINT('Ctrl Pts',(71.7847346627427,-69.885789325151,-419.974938351022));
#36803=CARTESIAN_POINT('Ctrl Pts',(71.7777818354168,-69.8862200417827,-419.984638846289));
#36804=CARTESIAN_POINT('Ctrl Pts',(66.0327739241091,-70.2421141752859,-427.99999999998));
#36805=CARTESIAN_POINT('Ctrl Pts',(66.0258284570958,-70.2425444359578,-428.009690226233));
#36806=CARTESIAN_POINT('Ctrl Pts',(71.7847226693789,-69.8886934082369,-419.974938351022));
#36807=CARTESIAN_POINT('Ctrl Pts',(71.7777669938073,-69.8891238150166,-419.984638846289));
#36808=CARTESIAN_POINT('Ctrl Pts',(66.030405623535,-70.2447619228682,-427.99999999998));
#36809=CARTESIAN_POINT('Ctrl Pts',(66.0234573112912,-70.2451918740163,-428.009690226233));
#36810=CARTESIAN_POINT('',(71.2680022706319,-61.2374772862763,-427.999999999981));
#36811=CARTESIAN_POINT('Ctrl Pts',(71.2680022706319,-61.2374772862763,-427.999999999981));
#36812=CARTESIAN_POINT('Ctrl Pts',(70.7169686230221,-62.8824630892616,-427.999999999984));
#36813=CARTESIAN_POINT('Ctrl Pts',(69.9924483273882,-64.4883621667366,-427.999999999984));
#36814=CARTESIAN_POINT('Ctrl Pts',(68.2308187876944,-67.5193402102828,-427.999999999984));
#36815=CARTESIAN_POINT('Ctrl Pts',(67.1940828116548,-68.9437769487187,-427.999999999983));
#36816=CARTESIAN_POINT('Ctrl Pts',(66.0375105251256,-70.2368186801723,-427.99999999998));
#36817=CARTESIAN_POINT('',(71.7785821060487,-69.7241904101463,-419.984638846392));
#36818=CARTESIAN_POINT('Ctrl Pts',(71.778582106068,-69.7241904101441,-419.984638846374));
#36819=CARTESIAN_POINT('Ctrl Pts',(71.7724644689808,-69.5879398537705,-419.994300721347));
#36820=CARTESIAN_POINT('Ctrl Pts',(71.7663297925677,-69.4514997697602,-420.004464228877));
#36821=CARTESIAN_POINT('Ctrl Pts',(71.6665242759986,-67.2352993224928,-420.178695493911));
#36822=CARTESIAN_POINT('Ctrl Pts',(71.60056809321,-65.8216385836969,-420.421054474862));
#36823=CARTESIAN_POINT('Ctrl Pts',(71.5182723428083,-64.1845886707567,-421.040376650859));
#36824=CARTESIAN_POINT('Ctrl Pts',(71.4918603696667,-63.6955909228312,-421.330095000737));
#36825=CARTESIAN_POINT('Ctrl Pts',(71.4436586475032,-62.8895206864909,-422.074609843585));
#36826=CARTESIAN_POINT('Ctrl Pts',(71.4213410766748,-62.5645635997133,-422.539913205919));
#36827=CARTESIAN_POINT('Ctrl Pts',(71.3770638450802,-62.0257982080005,-423.727790377744));
#36828=CARTESIAN_POINT('Ctrl Pts',(71.354594264779,-61.8059481386615,-424.464451567814));
#36829=CARTESIAN_POINT('Ctrl Pts',(71.3080373014504,-61.4528374554223,-426.246752571476));
#36830=CARTESIAN_POINT('Ctrl Pts',(71.2860320806886,-61.3272098966048,-427.192293569671));
#36831=CARTESIAN_POINT('Ctrl Pts',(71.2680022706313,-61.2374772862774,-427.999999999981));
#36832=CARTESIAN_POINT('Origin',(64.4008420083176,-77.3577815719416,-409.614647527464));
#36833=CARTESIAN_POINT('Ctrl Pts',(71.7845769902984,47.5507006514563,-419.975141527627));
#36834=CARTESIAN_POINT('Ctrl Pts',(71.7777670028513,47.5511220435636,-419.984638846302));
#36835=CARTESIAN_POINT('Ctrl Pts',(66.0304070683082,47.9067603076004,-427.999999999993));
#36836=CARTESIAN_POINT('Ctrl Pts',(66.0236629564188,47.9071776234241,-428.009405447549));
#36837=CARTESIAN_POINT('Ctrl Pts',(71.7845890408676,47.5477971654049,-419.975141527627));
#36838=CARTESIAN_POINT('Ctrl Pts',(71.7777818414427,47.5482188608126,-419.984638846302));
#36839=CARTESIAN_POINT('Ctrl Pts',(66.0327748872881,47.9041130984382,-427.999999999993));
#36840=CARTESIAN_POINT('Ctrl Pts',(66.0260335364513,47.9045307146284,-428.009405447549));
#36841=CARTESIAN_POINT('Ctrl Pts',(71.7846010914369,47.5448936793535,-419.975141527627));
#36842=CARTESIAN_POINT('Ctrl Pts',(71.7777966800341,47.5453156780617,-419.984638846302));
#36843=CARTESIAN_POINT('Ctrl Pts',(66.0351427062678,47.901465889276,-427.999999999993));
#36844=CARTESIAN_POINT('Ctrl Pts',(66.0284041164837,47.9018838058327,-428.009405447549));
#36845=CARTESIAN_POINT('Ctrl Pts',(71.7846131420061,47.5419901933021,-419.975141527627));
#36846=CARTESIAN_POINT('Ctrl Pts',(71.7778115186255,47.5424124953107,-419.984638846302));
#36847=CARTESIAN_POINT('Ctrl Pts',(66.0375105252477,47.8988186801138,-427.999999999993));
#36848=CARTESIAN_POINT('Ctrl Pts',(66.0307746965162,47.899236897037,-428.009405447549));
#36849=CARTESIAN_POINT('Ctrl Pts',(71.7904992990764,46.1237688133607,-419.975141527627));
#36850=CARTESIAN_POINT('Ctrl Pts',(71.7850594982006,46.1243392639028,-419.984638846302));
#36851=CARTESIAN_POINT('Ctrl Pts',(67.1940828116472,46.6057769487113,-427.999999999993));
#36852=CARTESIAN_POINT('Ctrl Pts',(67.1886956320016,46.6063418810718,-428.009405447549));
#36853=CARTESIAN_POINT('Ctrl Pts',(71.7896867258443,44.698202583494,-419.975141527626));
#36854=CARTESIAN_POINT('Ctrl Pts',(71.7854748505759,44.6987743707749,-419.984638846302));
#36855=CARTESIAN_POINT('Ctrl Pts',(68.2308187876864,45.1813402102757,-427.999999999993));
#36856=CARTESIAN_POINT('Ctrl Pts',(68.2266476554641,45.1819064664442,-428.009405447549));
#36857=CARTESIAN_POINT('Ctrl Pts',(71.7706298993564,41.8368906599961,-419.975141527626));
#36858=CARTESIAN_POINT('Ctrl Pts',(71.7685254439183,41.8372616495662,-419.984638846302));
#36859=CARTESIAN_POINT('Ctrl Pts',(69.9924483273799,42.1503621667298,-427.999999999992));
#36860=CARTESIAN_POINT('Ctrl Pts',(69.9903642291271,42.1507295675789,-428.009405447548));
#36861=CARTESIAN_POINT('Ctrl Pts',(71.7523647807903,40.4011808662495,-419.975141527626));
#36862=CARTESIAN_POINT('Ctrl Pts',(71.7511394025111,40.4013504389513,-419.984638846301));
#36863=CARTESIAN_POINT('Ctrl Pts',(70.7169686230137,40.5444630892552,-427.999999999992));
#36864=CARTESIAN_POINT('Ctrl Pts',(70.7157550982773,40.5446310216167,-428.009405447548));
#36865=CARTESIAN_POINT('Ctrl Pts',(71.7244019315222,38.9632861635067,-419.975141527626));
#36866=CARTESIAN_POINT('Ctrl Pts',(71.7238617882864,38.9632106465062,-419.984638846301));
#36867=CARTESIAN_POINT('Ctrl Pts',(71.2680022706226,38.8994772862712,-427.999999999992));
#36868=CARTESIAN_POINT('Ctrl Pts',(71.2674673523943,38.899402499775,-428.009405447548));
#36869=CARTESIAN_POINT('Ctrl Pts',(71.7243772829291,38.9620186931902,-419.975141527626));
#36870=CARTESIAN_POINT('Ctrl Pts',(71.7238377437118,38.9619429601488,-419.984638846301));
#36871=CARTESIAN_POINT('Ctrl Pts',(71.2684879938055,38.8980272700272,-427.999999999992));
#36872=CARTESIAN_POINT('Ctrl Pts',(71.2679536737529,38.8979522695799,-428.009405447548));
#36873=CARTESIAN_POINT('Ctrl Pts',(71.7243526343361,38.9607512228738,-419.975141527626));
#36874=CARTESIAN_POINT('Ctrl Pts',(71.7238136991373,38.9606752737917,-419.984638846301));
#36875=CARTESIAN_POINT('Ctrl Pts',(71.2689737169883,38.8965772537831,-427.999999999992));
#36876=CARTESIAN_POINT('Ctrl Pts',(71.2684399951114,38.8965020393849,-428.009405447549));
#36877=CARTESIAN_POINT('Ctrl Pts',(71.724327985743,38.9594837525574,-419.975141527626));
#36878=CARTESIAN_POINT('Ctrl Pts',(71.7237896545628,38.9594075874345,-419.984638846301));
#36879=CARTESIAN_POINT('Ctrl Pts',(71.2694594401712,38.8951272375391,-427.999999999992));
#36880=CARTESIAN_POINT('Ctrl Pts',(71.2689263164701,38.8950518091899,-428.009405447549));
#36881=CARTESIAN_POINT('',(71.6057458573101,47.5530957793322,-420.224899491064));
#36882=CARTESIAN_POINT('',(66.0375105252219,47.898818680116,-427.999999999993));
#36883=CARTESIAN_POINT('',(68.8215314165122,47.7259632383151,-424.112584875133));
#36884=CARTESIAN_POINT('',(71.7786391684187,47.3861353502518,-419.984557726008));
#36885=CARTESIAN_POINT('Origin',(64.4003613790409,55.0197702565038,-409.614309286759));
#36886=CARTESIAN_POINT('',(71.2658001249267,38.9060482850192,-428.000000003827));
#36887=CARTESIAN_POINT('Ctrl Pts',(71.2658001318634,38.9060483074633,-428.000000006487));
#36888=CARTESIAN_POINT('Ctrl Pts',(71.2847793839212,39.0007231868482,-427.151708897607));
#36889=CARTESIAN_POINT('Ctrl Pts',(71.306654613254,39.1265604842562,-426.216057544933));
#36890=CARTESIAN_POINT('Ctrl Pts',(71.3535698042164,39.4855033680191,-424.433577913956));
#36891=CARTESIAN_POINT('Ctrl Pts',(71.3760120589591,39.706267418997,-423.704408309738));
#36892=CARTESIAN_POINT('Ctrl Pts',(71.4203644905395,40.2470716344453,-422.526424835325));
#36893=CARTESIAN_POINT('Ctrl Pts',(71.4427828497872,40.5733100297556,-422.064118343691));
#36894=CARTESIAN_POINT('Ctrl Pts',(71.4914697497189,41.3852894835831,-421.320566931233));
#36895=CARTESIAN_POINT('Ctrl Pts',(71.5183087371882,41.8804392463264,-421.030345873091));
#36896=CARTESIAN_POINT('Ctrl Pts',(71.6043042830006,43.5837088832162,-420.394309344988));
#36897=CARTESIAN_POINT('Ctrl Pts',(71.67321649527,45.0589041174777,-420.162231586715));
#36898=CARTESIAN_POINT('Ctrl Pts',(71.7699783245184,47.1946696740857,-419.99846094143));
#36899=CARTESIAN_POINT('Ctrl Pts',(71.7743121912236,47.2904318327341,-419.991385923449));
#36900=CARTESIAN_POINT('Ctrl Pts',(71.7786391684188,47.3861353502518,-419.984557726009));
#36901=CARTESIAN_POINT('Ctrl Pts',(66.0375105252324,47.8988186801254,-428.));
#36902=CARTESIAN_POINT('Ctrl Pts',(67.1940828116486,46.605776948712,-427.999999999994));
#36903=CARTESIAN_POINT('Ctrl Pts',(68.2308187876859,45.1813402102759,-427.999999999994));
#36904=CARTESIAN_POINT('Ctrl Pts',(69.1116335575328,43.6658511885029,-427.999999999994));
#36905=CARTESIAN_POINT('Ctrl Pts',(69.9912754750915,42.1523801219546,-427.999999999994));
#36906=CARTESIAN_POINT('Ctrl Pts',(70.7150388674181,40.5487396111317,-428.00000000066));
#36907=CARTESIAN_POINT('Ctrl Pts',(71.2658001433482,38.9060482734612,-428.000000005073));
#36908=CARTESIAN_POINT('Ctrl Pts',(58.7165065275772,60.4445253144006,-420.221597501103));
#36909=CARTESIAN_POINT('Ctrl Pts',(58.7166543483028,60.4421594297898,-420.224899490944));
#36910=CARTESIAN_POINT('Ctrl Pts',(59.0647235592219,54.8712789827216,-427.999999999994));
#36911=CARTESIAN_POINT('Ctrl Pts',(59.0648834786915,54.8687194565731,-428.003572249165));
#36912=CARTESIAN_POINT('Ctrl Pts',(58.7183206700676,60.4427204158123,-420.221597501103));
#36913=CARTESIAN_POINT('Ctrl Pts',(58.7184681586435,60.4403549056508,-420.224899490944));
#36914=CARTESIAN_POINT('Ctrl Pts',(59.0657552661854,54.8703561635636,-427.999999999994));
#36915=CARTESIAN_POINT('Ctrl Pts',(59.0659148263198,54.8677970425123,-428.003572249165));
#36916=CARTESIAN_POINT('Ctrl Pts',(58.7201348125581,60.4409155172241,-420.221597501103));
#36917=CARTESIAN_POINT('Ctrl Pts',(58.7202819689841,60.4385503815119,-420.224899490944));
#36918=CARTESIAN_POINT('Ctrl Pts',(59.0667869731489,54.8694333444057,-427.999999999994));
#36919=CARTESIAN_POINT('Ctrl Pts',(59.0669461739481,54.8668746284513,-428.003572249165));
#36920=CARTESIAN_POINT('Ctrl Pts',(58.7219489550484,60.4391106186359,-420.221597501103));
#36921=CARTESIAN_POINT('Ctrl Pts',(58.7220957793248,60.436745857373,-420.224899490944));
#36922=CARTESIAN_POINT('Ctrl Pts',(59.0678186801124,54.8685105252478,-427.999999999994));
#36923=CARTESIAN_POINT('Ctrl Pts',(59.0679775215763,54.8659522143904,-428.003572249165));
#36924=CARTESIAN_POINT('Ctrl Pts',(60.8749752248954,58.2970550218832,-420.221597501103));
#36925=CARTESIAN_POINT('Ctrl Pts',(60.8747278535326,58.2951346574465,-420.224899490944));
#36926=CARTESIAN_POINT('Ctrl Pts',(60.2922496203792,53.7733077504804,-427.999999999994));
#36927=CARTESIAN_POINT('Ctrl Pts',(60.2919820023102,53.7712302091802,-428.003572249165));
#36928=CARTESIAN_POINT('Ctrl Pts',(63.0254878424152,56.1520277409106,-420.221597501103));
#36929=CARTESIAN_POINT('Ctrl Pts',(63.0248347730807,56.1505381750392,-420.224899490944));
#36930=CARTESIAN_POINT('Ctrl Pts',(61.4870711942792,52.64310025933,-427.999999999994));
#36931=CARTESIAN_POINT('Ctrl Pts',(61.4863646729084,52.6414887763439,-428.003572249165));
#36932=CARTESIAN_POINT('Ctrl Pts',(67.3210277409081,51.8564878424186,-420.221597501103));
#36933=CARTESIAN_POINT('Ctrl Pts',(67.3195381750366,51.8558347730841,-420.224899490943));
#36934=CARTESIAN_POINT('Ctrl Pts',(63.8121002593296,50.3180711942801,-427.999999999994));
#36935=CARTESIAN_POINT('Ctrl Pts',(63.8104887763433,50.3173646729094,-428.003572249165));
#36936=CARTESIAN_POINT('Ctrl Pts',(69.4660550218811,49.7059752248992,-420.221597501103));
#36937=CARTESIAN_POINT('Ctrl Pts',(69.4641346574443,49.7057278535363,-420.224899490943));
#36938=CARTESIAN_POINT('Ctrl Pts',(64.94230775048,49.1232496203804,-427.999999999994));
#36939=CARTESIAN_POINT('Ctrl Pts',(64.9402302091799,49.1229820023112,-428.003572249164));
#36940=CARTESIAN_POINT('Ctrl Pts',(71.6081106186342,47.5529489550527,-420.221597501102));
#36941=CARTESIAN_POINT('Ctrl Pts',(71.6057458573713,47.5530957793291,-420.224899490943));
#36942=CARTESIAN_POINT('Ctrl Pts',(66.0375105252477,47.8988186801138,-427.999999999993));
#36943=CARTESIAN_POINT('Ctrl Pts',(66.0349522143902,47.8989775215776,-428.003572249164));
#36944=CARTESIAN_POINT('Ctrl Pts',(71.6099155172282,47.5511348125565,-420.221597501102));
#36945=CARTESIAN_POINT('Ctrl Pts',(71.607550381516,47.5512819689826,-420.224899490943));
#36946=CARTESIAN_POINT('Ctrl Pts',(66.0384333444085,47.8977869731469,-427.999999999993));
#36947=CARTESIAN_POINT('Ctrl Pts',(66.0358746284541,47.897946173946,-428.003572249164));
#36948=CARTESIAN_POINT('Ctrl Pts',(71.6117204158223,47.5493206700602,-420.221597501102));
#36949=CARTESIAN_POINT('Ctrl Pts',(71.6093549056608,47.5494681586361,-420.224899490943));
#36950=CARTESIAN_POINT('Ctrl Pts',(66.0393561635695,47.8967552661801,-427.999999999993));
#36951=CARTESIAN_POINT('Ctrl Pts',(66.0367970425181,47.8969148263145,-428.003572249164));
#36952=CARTESIAN_POINT('Ctrl Pts',(71.6135253144163,47.5475065275639,-420.221597501102));
#36953=CARTESIAN_POINT('Ctrl Pts',(71.6111594298055,47.5476543482895,-420.224899490943));
#36954=CARTESIAN_POINT('Ctrl Pts',(66.0402789827303,47.8957235592132,-427.999999999993));
#36955=CARTESIAN_POINT('Ctrl Pts',(66.037719456582,47.8958834786829,-428.003572249164));
#36956=CARTESIAN_POINT('',(58.7220957792977,60.4367458573386,-420.224899491211));
#36957=CARTESIAN_POINT('',(59.0678186801968,54.8685105250433,-427.999999999994));
#36958=CARTESIAN_POINT('',(58.8896451722718,57.7381845310678,-423.992984762199));
#36959=CARTESIAN_POINT('Ctrl Pts',(71.6057458573105,47.5530957793328,-420.224899491028));
#36960=CARTESIAN_POINT('Ctrl Pts',(71.5788313549573,47.5800050273333,-420.225112345486));
#36961=CARTESIAN_POINT('Ctrl Pts',(71.3433705542102,47.815420487381,-420.226949102679));
#36962=CARTESIAN_POINT('Ctrl Pts',(71.0675267615548,48.0912133341899,-420.229012925044));
#36963=CARTESIAN_POINT('Ctrl Pts',(70.933028253816,48.2256877198568,-420.229990113084));
#36964=CARTESIAN_POINT('Ctrl Pts',(70.5296622520642,48.6289835944733,-420.232830971772));
#36965=CARTESIAN_POINT('Ctrl Pts',(70.2608984859449,48.8977035865951,-420.234604261675));
#36966=CARTESIAN_POINT('Ctrl Pts',(69.4547425199343,49.7037375567473,-420.239546328577));
#36967=CARTESIAN_POINT('Ctrl Pts',(68.9182881782743,50.2401231051503,-420.242333151697));
#36968=CARTESIAN_POINT('Ctrl Pts',(67.305913743342,51.8523309309769,-420.249082506609));
#36969=CARTESIAN_POINT('Ctrl Pts',(66.2386375096525,52.9195503715613,-420.251383202126));
#36970=CARTESIAN_POINT('Ctrl Pts',(64.0885415293445,55.0696463522429,-420.251383186968));
#36971=CARTESIAN_POINT('Ctrl Pts',(63.0213238305098,56.1369208443656,-420.249082484032));
#36972=CARTESIAN_POINT('Ctrl Pts',(61.409118673553,57.7492926104162,-420.242333129574));
#36973=CARTESIAN_POINT('Ctrl Pts',(60.8727340072911,58.2857460698852,-420.239546308474));
#36974=CARTESIAN_POINT('Ctrl Pts',(60.0667013674838,59.0919007054106,-420.23460424724));
#36975=CARTESIAN_POINT('Ctrl Pts',(59.7979818185451,59.3606640282894,-420.232830959659));
#36976=CARTESIAN_POINT('Ctrl Pts',(59.3946866092094,59.7640293646592,-420.229990105064));
#36977=CARTESIAN_POINT('Ctrl Pts',(59.2602124453863,59.898527650518,-420.229012918491));
#36978=CARTESIAN_POINT('Ctrl Pts',(58.9844329063737,60.1743581329234,-420.226949195513));
#36979=CARTESIAN_POINT('Ctrl Pts',(58.7490391213161,60.4097972543148,-420.225112615174));
#36980=CARTESIAN_POINT('Ctrl Pts',(58.7220957793007,60.4367458573401,-420.224899491029));
#36981=CARTESIAN_POINT('Origin',(31.3096343625947,20.140634036236,-428.000000005605));
#36982=CARTESIAN_POINT('Ctrl Pts',(52.3339462257355,60.6512190129386,-419.982643458044));
#36983=CARTESIAN_POINT('Ctrl Pts',(52.3338974363804,60.6510302761279,-419.985958630343));
#36984=CARTESIAN_POINT('Ctrl Pts',(52.2159548757098,60.194781106073,-427.999999999994));
#36985=CARTESIAN_POINT('Ctrl Pts',(52.215905926027,60.19459174905,-428.003326066353));
#36986=CARTESIAN_POINT('Ctrl Pts',(52.3347807659306,60.6512172558263,-419.982643458044));
#36987=CARTESIAN_POINT('Ctrl Pts',(52.3347320200057,60.651028258566,-419.985958630343));
#36988=CARTESIAN_POINT('Ctrl Pts',(52.2168944466177,60.1941494822845,-427.999999999994));
#36989=CARTESIAN_POINT('Ctrl Pts',(52.2168455405077,60.1939598639562,-428.003326066353));
#36990=CARTESIAN_POINT('Ctrl Pts',(52.3356153061257,60.6512154987138,-419.982643458044));
#36991=CARTESIAN_POINT('Ctrl Pts',(52.335566603631,60.6510262410041,-419.985958630343));
#36992=CARTESIAN_POINT('Ctrl Pts',(52.2178340175256,60.1935178584959,-427.999999999994));
#36993=CARTESIAN_POINT('Ctrl Pts',(52.2177851549885,60.1933279788623,-428.003326066353));
#36994=CARTESIAN_POINT('Ctrl Pts',(52.3364498463208,60.6512137416015,-419.982643458044));
#36995=CARTESIAN_POINT('Ctrl Pts',(52.3364011872562,60.6510242234422,-419.985958630343));
#36996=CARTESIAN_POINT('Ctrl Pts',(52.2187735884335,60.1928862347074,-427.999999999994));
#36997=CARTESIAN_POINT('Ctrl Pts',(52.2187247694692,60.1926960937683,-428.003326066353));
#36998=CARTESIAN_POINT('Ctrl Pts',(53.4022460080427,60.648969723097,-419.982643458044));
#36999=CARTESIAN_POINT('Ctrl Pts',(53.4022528138625,60.6484475833501,-419.985958630343));
#37000=CARTESIAN_POINT('Ctrl Pts',(53.4187050874362,59.3862358020305,-427.999999999994));
#37001=CARTESIAN_POINT('Ctrl Pts',(53.4187119156207,59.3857119464688,-428.003326066353));
#37002=CARTESIAN_POINT('Ctrl Pts',(54.4665375661037,60.6443135760932,-419.982643458044));
#37003=CARTESIAN_POINT('Ctrl Pts',(54.4665894999893,60.6434422462875,-419.985958630343));
#37004=CARTESIAN_POINT('Ctrl Pts',(54.5921335951925,58.5371043305541,-427.999999999994));
#37005=CARTESIAN_POINT('Ctrl Pts',(54.592185699739,58.5362301374525,-428.003326066353));
#37006=CARTESIAN_POINT('Ctrl Pts',(56.5916495236165,60.6305361381316,-419.982643458044));
#37007=CARTESIAN_POINT('Ctrl Pts',(56.5917678710043,60.6289357581116,-419.985958630343));
#37008=CARTESIAN_POINT('Ctrl Pts',(56.8778588421339,56.7602042011328,-427.999999999994));
#37009=CARTESIAN_POINT('Ctrl Pts',(56.8779775784257,56.7585985620691,-428.003326066352));
#37010=CARTESIAN_POINT('Ctrl Pts',(57.6524699230681,60.621414847174,-419.982643458044));
#37011=CARTESIAN_POINT('Ctrl Pts',(57.6526095558927,60.6194346069985,-419.985958630343));
#37012=CARTESIAN_POINT('Ctrl Pts',(57.990155581319,55.832435543188,-427.999999999994));
#37013=CARTESIAN_POINT('Ctrl Pts',(57.9902956729941,55.8304487957018,-428.003326066352));
#37014=CARTESIAN_POINT('Ctrl Pts',(58.711323769583,60.6102405408494,-419.982643458044));
#37015=CARTESIAN_POINT('Ctrl Pts',(58.7114711800225,60.607866338805,-419.985958630343));
#37016=CARTESIAN_POINT('Ctrl Pts',(59.0678186801124,54.8685105252478,-427.999999999994));
#37017=CARTESIAN_POINT('Ctrl Pts',(59.0679665749608,54.8661285212862,-428.003326066352));
#37018=CARTESIAN_POINT('Ctrl Pts',(58.7119775738259,60.6102336411164,-419.982643458044));
#37019=CARTESIAN_POINT('Ctrl Pts',(58.7121249890678,60.6078591958146,-419.985958630343));
#37020=CARTESIAN_POINT('Ctrl Pts',(59.0684840983935,54.8679153361491,-427.999999999994));
#37021=CARTESIAN_POINT('Ctrl Pts',(59.0686319980599,54.8655330881308,-428.003326066352));
#37022=CARTESIAN_POINT('Ctrl Pts',(58.7126313780688,60.6102267413832,-419.982643458044));
#37023=CARTESIAN_POINT('Ctrl Pts',(58.7127787981132,60.6078520528242,-419.985958630343));
#37024=CARTESIAN_POINT('Ctrl Pts',(59.0691495166747,54.8673201470504,-427.999999999994));
#37025=CARTESIAN_POINT('Ctrl Pts',(59.0692974211592,54.8649376549753,-428.003326066352));
#37026=CARTESIAN_POINT('Ctrl Pts',(58.7132851823118,60.6102198416502,-419.982643458044));
#37027=CARTESIAN_POINT('Ctrl Pts',(58.7134326071585,60.6078449098338,-419.985958630343));
#37028=CARTESIAN_POINT('Ctrl Pts',(59.0698149349556,54.8667249579515,-427.999999999994));
#37029=CARTESIAN_POINT('Ctrl Pts',(59.0699628442584,54.8643422218199,-428.003326066352));
#37030=CARTESIAN_POINT('',(52.2187735884339,60.1928862347074,-427.999999999994));
#37031=CARTESIAN_POINT('Origin',(36.4516651763393,32.8363615764921,-427.999999997771));
#37032=CARTESIAN_POINT('',(58.5551812881547,60.6095586489222,-419.985958630427));
#37033=CARTESIAN_POINT('Ctrl Pts',(58.5551812881547,60.6095586489222,-419.985958630428));
#37034=CARTESIAN_POINT('Ctrl Pts',(57.8905656231904,60.579613056112,-420.039064310979));
#37035=CARTESIAN_POINT('Ctrl Pts',(57.1413284898495,60.5455711556876,-420.115158862097));
#37036=CARTESIAN_POINT('Ctrl Pts',(55.795021970294,60.4827534710867,-420.346199566438));
#37037=CARTESIAN_POINT('Ctrl Pts',(55.2653957129864,60.4571327211903,-420.489103173694));
#37038=CARTESIAN_POINT('Ctrl Pts',(54.4868753060455,60.4174201214811,-420.816585135814));
#37039=CARTESIAN_POINT('Ctrl Pts',(54.1948026574575,60.4016105264185,-420.991578345459));
#37040=CARTESIAN_POINT('Ctrl Pts',(53.6669859901669,60.3705778942932,-421.448755462825));
#37041=CARTESIAN_POINT('Ctrl Pts',(53.4423116413425,60.3556681374191,-421.74067122796));
#37042=CARTESIAN_POINT('Ctrl Pts',(52.9255518670193,60.3157041841555,-422.736667045547));
#37043=CARTESIAN_POINT('Ctrl Pts',(52.7154746644318,60.2918022892675,-423.579729317975));
#37044=CARTESIAN_POINT('Ctrl Pts',(52.4080044297822,60.2427721479772,-425.617637073544));
#37045=CARTESIAN_POINT('Ctrl Pts',(52.3028359111884,60.2177714544809,-426.785751435106));
#37046=CARTESIAN_POINT('Ctrl Pts',(52.2187735884335,60.1928862347074,-427.999999999994));
#37047=CARTESIAN_POINT('Origin',(65.4233329644767,53.9721173749241,-410.627910492205));
#37048=CARTESIAN_POINT('Ctrl Pts',(-52.3339462257464,60.6512190129295,-419.982643458044));
#37049=CARTESIAN_POINT('Ctrl Pts',(-52.3338974363913,60.6510302761188,-419.985958630342));
#37050=CARTESIAN_POINT('Ctrl Pts',(-52.2159548757207,60.1947811060639,-427.999999999992));
#37051=CARTESIAN_POINT('Ctrl Pts',(-52.2159059260379,60.1945917490409,-428.003326066352));
#37052=CARTESIAN_POINT('Ctrl Pts',(-52.3347807659415,60.6512172558172,-419.982643458044));
#37053=CARTESIAN_POINT('Ctrl Pts',(-52.3347320200165,60.6510282585569,-419.985958630342));
#37054=CARTESIAN_POINT('Ctrl Pts',(-52.2168944466286,60.1941494822754,-427.999999999992));
#37055=CARTESIAN_POINT('Ctrl Pts',(-52.2168455405186,60.1939598639471,-428.003326066352));
#37056=CARTESIAN_POINT('Ctrl Pts',(-52.3356153061366,60.6512154987047,-419.982643458044));
#37057=CARTESIAN_POINT('Ctrl Pts',(-52.3355666036418,60.651026240995,-419.985958630342));
#37058=CARTESIAN_POINT('Ctrl Pts',(-52.2178340175365,60.1935178584868,-427.999999999992));
#37059=CARTESIAN_POINT('Ctrl Pts',(-52.2177851549993,60.1933279788531,-428.003326066352));
#37060=CARTESIAN_POINT('Ctrl Pts',(-52.3364498463317,60.6512137415924,-419.982643458044));
#37061=CARTESIAN_POINT('Ctrl Pts',(-52.336401187267,60.6510242234331,-419.985958630342));
#37062=CARTESIAN_POINT('Ctrl Pts',(-52.2187735884443,60.1928862346983,-427.999999999992));
#37063=CARTESIAN_POINT('Ctrl Pts',(-52.2187247694801,60.1926960937592,-428.003326066352));
#37064=CARTESIAN_POINT('Ctrl Pts',(-53.4022460080535,60.6489697230877,-419.982643458044));
#37065=CARTESIAN_POINT('Ctrl Pts',(-53.4022528138733,60.6484475833408,-419.985958630342));
#37066=CARTESIAN_POINT('Ctrl Pts',(-53.418705087447,59.3862358020211,-427.999999999992));
#37067=CARTESIAN_POINT('Ctrl Pts',(-53.4187119156315,59.3857119464594,-428.003326066352));
#37068=CARTESIAN_POINT('Ctrl Pts',(-54.4665375661146,60.6443135760836,-419.982643458044));
#37069=CARTESIAN_POINT('Ctrl Pts',(-54.4665895,60.6434422462781,-419.985958630342));
#37070=CARTESIAN_POINT('Ctrl Pts',(-54.5921335952031,58.5371043305445,-427.999999999992));
#37071=CARTESIAN_POINT('Ctrl Pts',(-54.5921856997496,58.536230137443,-428.003326066352));
#37072=CARTESIAN_POINT('Ctrl Pts',(-56.5916495236273,60.6305361381218,-419.982643458044));
#37073=CARTESIAN_POINT('Ctrl Pts',(-56.5917678710151,60.6289357581018,-419.985958630342));
#37074=CARTESIAN_POINT('Ctrl Pts',(-56.8778588421441,56.760204201123,-427.999999999992));
#37075=CARTESIAN_POINT('Ctrl Pts',(-56.8779775784359,56.7585985620592,-428.003326066351));
#37076=CARTESIAN_POINT('Ctrl Pts',(-57.652469923079,60.6214148471639,-419.982643458044));
#37077=CARTESIAN_POINT('Ctrl Pts',(-57.6526095559036,60.6194346069884,-419.985958630342));
#37078=CARTESIAN_POINT('Ctrl Pts',(-57.9901555813291,55.8324355431779,-427.999999999992));
#37079=CARTESIAN_POINT('Ctrl Pts',(-57.9902956730042,55.8304487956918,-428.003326066351));
#37080=CARTESIAN_POINT('Ctrl Pts',(-58.7113237695938,60.6102405408391,-419.982643458044));
#37081=CARTESIAN_POINT('Ctrl Pts',(-58.7114711800333,60.6078663387948,-419.985958630342));
#37082=CARTESIAN_POINT('Ctrl Pts',(-59.0678186801224,54.8685105252375,-427.999999999992));
#37083=CARTESIAN_POINT('Ctrl Pts',(-59.0679665749706,54.8661285212758,-428.003326066351));
#37084=CARTESIAN_POINT('Ctrl Pts',(-58.7119775738368,60.6102336411061,-419.982643458044));
#37085=CARTESIAN_POINT('Ctrl Pts',(-58.7121249890787,60.6078591958044,-419.985958630342));
#37086=CARTESIAN_POINT('Ctrl Pts',(-59.0684840984036,54.8679153361386,-427.999999999992));
#37087=CARTESIAN_POINT('Ctrl Pts',(-59.06863199807,54.8655330881203,-428.003326066351));
#37088=CARTESIAN_POINT('Ctrl Pts',(-58.7126313780798,60.610226741373,-419.982643458044));
#37089=CARTESIAN_POINT('Ctrl Pts',(-58.7127787981242,60.6078520528141,-419.985958630342));
#37090=CARTESIAN_POINT('Ctrl Pts',(-59.0691495166847,54.8673201470398,-427.999999999992));
#37091=CARTESIAN_POINT('Ctrl Pts',(-59.0692974211693,54.8649376549648,-428.003326066351));
#37092=CARTESIAN_POINT('Ctrl Pts',(-58.7132851823228,60.6102198416399,-419.982643458044));
#37093=CARTESIAN_POINT('Ctrl Pts',(-58.7134326071696,60.6078449098237,-419.985958630342));
#37094=CARTESIAN_POINT('Ctrl Pts',(-59.0698149349659,54.8667249579411,-427.999999999992));
#37095=CARTESIAN_POINT('Ctrl Pts',(-59.0699628442686,54.8643422218093,-428.003326066351));
#37096=CARTESIAN_POINT('',(-59.0678186801055,54.8685105255263,-427.999999999992));
#37097=CARTESIAN_POINT('',(-52.2187735884448,60.1928862346983,-427.999999999992));
#37098=CARTESIAN_POINT('Origin',(-36.4516627737165,32.8363581330575,-427.999999989399));
#37099=CARTESIAN_POINT('',(-58.7220957793505,60.4367458573009,-420.22489949061));
#37100=CARTESIAN_POINT('',(-58.8949632383227,57.6525314165029,-424.112584875133));
#37101=CARTESIAN_POINT('',(-58.5551812881654,60.609558648911,-419.985958630427));
#37102=CARTESIAN_POINT('Origin',(-65.4233332963058,53.9721185186547,-410.627911078019));
#37103=CARTESIAN_POINT('Ctrl Pts',(-52.2187735884443,60.1928862346983,-427.999999999992));
#37104=CARTESIAN_POINT('Ctrl Pts',(-52.3048068721005,60.2183549238976,-426.757281647839));
#37105=CARTESIAN_POINT('Ctrl Pts',(-52.4145242813431,60.2444171332054,-425.539778431885));
#37106=CARTESIAN_POINT('Ctrl Pts',(-52.7414645491196,60.2952148912895,-423.449355059722));
#37107=CARTESIAN_POINT('Ctrl Pts',(-52.9555637437187,60.3179344965143,-422.684012418721));
#37108=CARTESIAN_POINT('Ctrl Pts',(-53.4350583564631,60.3551633628339,-421.751436601779));
#37109=CARTESIAN_POINT('Ctrl Pts',(-53.6588138203951,60.3700593220912,-421.458014299146));
#37110=CARTESIAN_POINT('Ctrl Pts',(-54.1844910544222,60.401037189882,-420.998625299011));
#37111=CARTESIAN_POINT('Ctrl Pts',(-54.475305566902,60.4168068389036,-420.822774395234));
#37112=CARTESIAN_POINT('Ctrl Pts',(-55.2486929141825,60.4563082169502,-420.494554521714));
#37113=CARTESIAN_POINT('Ctrl Pts',(-55.7731969610708,60.4817083073866,-420.35148029123));
#37114=CARTESIAN_POINT('Ctrl Pts',(-57.1207377485714,60.5446364896661,-420.117199581875));
#37115=CARTESIAN_POINT('Ctrl Pts',(-57.8825166626905,60.5792503940301,-420.039707457912));
#37116=CARTESIAN_POINT('Ctrl Pts',(-58.5551812881653,60.609558648912,-419.985958630427));
#37117=CARTESIAN_POINT('Ctrl Pts',(-58.7165065275705,60.4445253144079,-420.221597501101));
#37118=CARTESIAN_POINT('Ctrl Pts',(-58.7166543482962,60.4421594297969,-420.224899490943));
#37119=CARTESIAN_POINT('Ctrl Pts',(-59.0647235592219,54.8712789827201,-427.999999999992));
#37120=CARTESIAN_POINT('Ctrl Pts',(-59.0648834786916,54.8687194565718,-428.003572249163));
#37121=CARTESIAN_POINT('Ctrl Pts',(-58.7183206700667,60.4427204158139,-420.221597501101));
#37122=CARTESIAN_POINT('Ctrl Pts',(-58.7184681586425,60.4403549056522,-420.224899490943));
#37123=CARTESIAN_POINT('Ctrl Pts',(-59.0657552661887,54.8703561635592,-427.999999999992));
#37124=CARTESIAN_POINT('Ctrl Pts',(-59.0659148263231,54.8677970425078,-428.003572249163));
#37125=CARTESIAN_POINT('Ctrl Pts',(-58.720134812563,60.4409155172199,-420.221597501101));
#37126=CARTESIAN_POINT('Ctrl Pts',(-58.720281968989,60.4385503815075,-420.224899490943));
#37127=CARTESIAN_POINT('Ctrl Pts',(-59.0667869731556,54.8694333443983,-427.999999999992));
#37128=CARTESIAN_POINT('Ctrl Pts',(-59.0669461739546,54.8668746284439,-428.003572249163));
#37129=CARTESIAN_POINT('Ctrl Pts',(-58.7219489550591,60.4391106186259,-420.221597501101));
#37130=CARTESIAN_POINT('Ctrl Pts',(-58.7220957793355,60.4367458573628,-420.224899490943));
#37131=CARTESIAN_POINT('Ctrl Pts',(-59.0678186801224,54.8685105252375,-427.999999999992));
#37132=CARTESIAN_POINT('Ctrl Pts',(-59.0679775215862,54.8659522143801,-428.003572249163));
#37133=CARTESIAN_POINT('Ctrl Pts',(-60.8749752249057,58.2970550218727,-420.221597501101));
#37134=CARTESIAN_POINT('Ctrl Pts',(-60.874727853543,58.2951346574359,-420.224899490943));
#37135=CARTESIAN_POINT('Ctrl Pts',(-60.292249620389,53.7733077504698,-427.999999999992));
#37136=CARTESIAN_POINT('Ctrl Pts',(-60.2919820023199,53.7712302091697,-428.003572249163));
#37137=CARTESIAN_POINT('Ctrl Pts',(-63.0254878424252,56.1520277408997,-420.221597501101));
#37138=CARTESIAN_POINT('Ctrl Pts',(-63.0248347730907,56.1505381750281,-420.224899490943));
#37139=CARTESIAN_POINT('Ctrl Pts',(-61.4870711942888,52.6431002593193,-427.999999999992));
#37140=CARTESIAN_POINT('Ctrl Pts',(-61.486364672918,52.6414887763331,-428.003572249163));
#37141=CARTESIAN_POINT('Ctrl Pts',(-67.3210277409174,51.8564878424069,-420.221597501101));
#37142=CARTESIAN_POINT('Ctrl Pts',(-67.3195381750458,51.8558347730723,-420.224899490942));
#37143=CARTESIAN_POINT('Ctrl Pts',(-63.8121002593388,50.3180711942689,-427.999999999992));
#37144=CARTESIAN_POINT('Ctrl Pts',(-63.8104887763525,50.3173646728982,-428.003572249163));
#37145=CARTESIAN_POINT('Ctrl Pts',(-69.46605502189,49.7059752248871,-420.221597501101));
#37146=CARTESIAN_POINT('Ctrl Pts',(-69.4641346574531,49.7057278535242,-420.224899490941));
#37147=CARTESIAN_POINT('Ctrl Pts',(-64.942307750489,49.123249620369,-427.999999999991));
#37148=CARTESIAN_POINT('Ctrl Pts',(-64.9402302091889,49.1229820022998,-428.003572249162));
#37149=CARTESIAN_POINT('Ctrl Pts',(-71.6081106186428,47.5529489550402,-420.2215975011));
#37150=CARTESIAN_POINT('Ctrl Pts',(-71.6057458573797,47.5530957793166,-420.224899490941));
#37151=CARTESIAN_POINT('Ctrl Pts',(-66.0375105252564,47.8988186801022,-427.999999999991));
#37152=CARTESIAN_POINT('Ctrl Pts',(-66.034952214399,47.898977521566,-428.003572249162));
#37153=CARTESIAN_POINT('Ctrl Pts',(-71.6099155172309,47.5511348125498,-420.2215975011));
#37154=CARTESIAN_POINT('Ctrl Pts',(-71.6075503815186,47.5512819689759,-420.224899490941));
#37155=CARTESIAN_POINT('Ctrl Pts',(-66.0384333444143,47.8977869731387,-427.999999999991));
#37156=CARTESIAN_POINT('Ctrl Pts',(-66.0358746284599,47.8979461739377,-428.003572249162));
#37157=CARTESIAN_POINT('Ctrl Pts',(-71.6117204158191,47.5493206700594,-420.2215975011));
#37158=CARTESIAN_POINT('Ctrl Pts',(-71.6093549056575,47.5494681586352,-420.224899490941));
#37159=CARTESIAN_POINT('Ctrl Pts',(-66.0393561635722,47.8967552661752,-427.999999999991));
#37160=CARTESIAN_POINT('Ctrl Pts',(-66.0367970425208,47.8969148263095,-428.003572249162));
#37161=CARTESIAN_POINT('Ctrl Pts',(-71.6135253144073,47.5475065275691,-420.2215975011));
#37162=CARTESIAN_POINT('Ctrl Pts',(-71.6111594297964,47.5476543482947,-420.224899490941));
#37163=CARTESIAN_POINT('Ctrl Pts',(-66.04027898273,47.8957235592116,-427.999999999991));
#37164=CARTESIAN_POINT('Ctrl Pts',(-66.0377194565817,47.8958834786813,-428.003572249162));
#37165=CARTESIAN_POINT('',(-66.0375105252203,47.8988186801189,-427.999999999992));
#37166=CARTESIAN_POINT('Origin',(-31.3096249078695,20.1406251047006,-427.999999986154));
#37167=CARTESIAN_POINT('',(-71.6057458573148,47.5530957793236,-420.224899491057));
#37168=CARTESIAN_POINT('',(-68.9076650111372,47.720615340018,-423.992313852913));
#37169=CARTESIAN_POINT('Ctrl Pts',(-58.7220957793437,60.4367458572975,-420.224899491029));
#37170=CARTESIAN_POINT('Ctrl Pts',(-58.7490050273443,60.4098313549443,-420.225112345487));
#37171=CARTESIAN_POINT('Ctrl Pts',(-58.9844219604456,60.1743690808714,-420.226949113703));
#37172=CARTESIAN_POINT('Ctrl Pts',(-59.2602133340583,59.8985267616844,-420.229012925044));
#37173=CARTESIAN_POINT('Ctrl Pts',(-59.394687719799,59.7640282538717,-420.229990113084));
#37174=CARTESIAN_POINT('Ctrl Pts',(-59.7979835947372,59.3606622517981,-420.232830971774));
#37175=CARTESIAN_POINT('Ctrl Pts',(-60.0667035867286,59.0918984858094,-420.234604261676));
#37176=CARTESIAN_POINT('Ctrl Pts',(-60.8727375567052,58.2857425199744,-420.239546328577));
#37177=CARTESIAN_POINT('Ctrl Pts',(-61.4091231051397,57.7492881782828,-420.242333151698));
#37178=CARTESIAN_POINT('Ctrl Pts',(-63.0213309310531,56.1369137432638,-420.249082506609));
#37179=CARTESIAN_POINT('Ctrl Pts',(-64.0885503716052,55.0696375096067,-420.251383202125));
#37180=CARTESIAN_POINT('Ctrl Pts',(-66.238646352251,52.9195415293347,-420.251383186966));
#37181=CARTESIAN_POINT('Ctrl Pts',(-67.3059208443576,51.852323830516,-420.249082484029));
#37182=CARTESIAN_POINT('Ctrl Pts',(-68.9182926103748,50.2401186735927,-420.242333129571));
#37183=CARTESIAN_POINT('Ctrl Pts',(-69.4547460697976,49.703734007377,-420.239546308471));
#37184=CARTESIAN_POINT('Ctrl Pts',(-70.2609007054035,48.8977013674892,-420.234604247237));
#37185=CARTESIAN_POINT('Ctrl Pts',(-70.5296640282886,48.6289818185442,-420.232830959655));
#37186=CARTESIAN_POINT('Ctrl Pts',(-70.9330293646132,48.2256866092536,-420.229990105061));
#37187=CARTESIAN_POINT('Ctrl Pts',(-71.0675276504441,48.0912124454586,-420.229012918488));
#37188=CARTESIAN_POINT('Ctrl Pts',(-71.3433692203882,47.8154218209551,-420.226949112555));
#37189=CARTESIAN_POINT('Ctrl Pts',(-71.5788313994088,47.5800049828864,-420.225112345133));
#37190=CARTESIAN_POINT('Ctrl Pts',(-71.605745857315,47.5530957793241,-420.224899491026));
#37191=CARTESIAN_POINT('Ctrl Pts',(-71.7845249352717,47.5507056437107,-419.975214114147));
#37192=CARTESIAN_POINT('Ctrl Pts',(-71.7777669938055,47.5511238150004,-419.984638846301));
#37193=CARTESIAN_POINT('Ctrl Pts',(-66.0304056235332,47.9067619228495,-427.999999999991));
#37194=CARTESIAN_POINT('Ctrl Pts',(-66.0236556702644,47.9071795998414,-428.009413591679));
#37195=CARTESIAN_POINT('Ctrl Pts',(-71.7845370096047,47.547801569433,-419.975214114147));
#37196=CARTESIAN_POINT('Ctrl Pts',(-71.777781835415,47.5482200417663,-419.984638846301));
#37197=CARTESIAN_POINT('Ctrl Pts',(-66.0327739241075,47.9041141752671,-427.999999999991));
#37198=CARTESIAN_POINT('Ctrl Pts',(-66.0260267348443,47.9045321529467,-428.009413591679));
#37199=CARTESIAN_POINT('Ctrl Pts',(-71.7845490839377,47.5448974951555,-419.975214114147));
#37200=CARTESIAN_POINT('Ctrl Pts',(-71.7777966770244,47.5453162685322,-419.984638846301));
#37201=CARTESIAN_POINT('Ctrl Pts',(-66.035142224682,47.9014664276846,-427.999999999991));
#37202=CARTESIAN_POINT('Ctrl Pts',(-66.0283977994242,47.9018847060521,-428.009413591679));
#37203=CARTESIAN_POINT('Ctrl Pts',(-71.7845611582707,47.5419934208777,-419.975214114147));
#37204=CARTESIAN_POINT('Ctrl Pts',(-71.7778115186339,47.5424124952982,-419.984638846301));
#37205=CARTESIAN_POINT('Ctrl Pts',(-66.0375105252564,47.8988186801022,-427.999999999991));
#37206=CARTESIAN_POINT('Ctrl Pts',(-66.0307688640041,47.8992372591574,-428.009413591679));
#37207=CARTESIAN_POINT('Ctrl Pts',(-71.7904577235372,46.1237731732124,-419.975214114147));
#37208=CARTESIAN_POINT('Ctrl Pts',(-71.7850594982088,46.1243392638902,-419.984638846301));
#37209=CARTESIAN_POINT('Ctrl Pts',(-67.1940828116557,46.6057769486995,-427.999999999991));
#37210=CARTESIAN_POINT('Ctrl Pts',(-67.1886909672778,46.6063423702321,-428.009413591679));
#37211=CARTESIAN_POINT('Ctrl Pts',(-71.7896545351483,44.6982069535623,-419.975214114147));
#37212=CARTESIAN_POINT('Ctrl Pts',(-71.7854748505838,44.6987743707624,-419.9846388463));
#37213=CARTESIAN_POINT('Ctrl Pts',(-68.2308187876946,45.1813402102638,-427.999999999991));
#37214=CARTESIAN_POINT('Ctrl Pts',(-68.2266440437095,45.1819069567506,-428.009413591679));
#37215=CARTESIAN_POINT('Ctrl Pts',(-71.77061381534,41.8368934953987,-419.975214114147));
#37216=CARTESIAN_POINT('Ctrl Pts',(-71.7685254439257,41.8372616495537,-419.9846388463));
#37217=CARTESIAN_POINT('Ctrl Pts',(-69.9924483273876,42.1503621667176,-427.999999999991));
#37218=CARTESIAN_POINT('Ctrl Pts',(-69.9903624245244,42.1507298856973,-428.009413591678));
#37219=CARTESIAN_POINT('Ctrl Pts',(-71.7523554154229,40.4011821622547,-419.975214114146));
#37220=CARTESIAN_POINT('Ctrl Pts',(-71.7511394025183,40.4013504389388,-419.9846388463));
#37221=CARTESIAN_POINT('Ctrl Pts',(-70.7169686230211,40.5444630892429,-427.99999999999));
#37222=CARTESIAN_POINT('Ctrl Pts',(-70.7157540474996,40.5446311670161,-428.009413591678));
#37223=CARTESIAN_POINT('Ctrl Pts',(-71.7243978032989,38.9632855863295,-419.975214114146));
#37224=CARTESIAN_POINT('Ctrl Pts',(-71.7238617882933,38.9632106464937,-419.9846388463));
#37225=CARTESIAN_POINT('Ctrl Pts',(-71.2680022706297,38.8994772862588,-427.99999999999));
#37226=CARTESIAN_POINT('Ctrl Pts',(-71.2674668892185,38.8994024350053,-428.009413591677));
#37227=CARTESIAN_POINT('Ctrl Pts',(-71.7243358633182,38.9600999320719,-419.975214114146));
#37228=CARTESIAN_POINT('Ctrl Pts',(-71.7238013548453,38.9600244533907,-419.9846388463));
#37229=CARTESIAN_POINT('Ctrl Pts',(-71.2692230835275,38.895832826626,-427.99999999999));
#37230=CARTESIAN_POINT('Ctrl Pts',(-71.2686892068682,38.8957574371642,-428.009413591677));
#37231=CARTESIAN_POINT('Ctrl Pts',(-71.7242739233376,38.9569142778141,-419.975214114145));
#37232=CARTESIAN_POINT('Ctrl Pts',(-71.7237409213973,38.9568382602878,-419.9846388463));
#37233=CARTESIAN_POINT('Ctrl Pts',(-71.2704438964254,38.8921883669931,-427.99999999999));
#37234=CARTESIAN_POINT('Ctrl Pts',(-71.2699115245179,38.892112439323,-428.009413591677));
#37235=CARTESIAN_POINT('Ctrl Pts',(-71.7242119833569,38.9537286235565,-419.975214114145));
#37236=CARTESIAN_POINT('Ctrl Pts',(-71.7236804879494,38.9536520671848,-419.9846388463));
#37237=CARTESIAN_POINT('Ctrl Pts',(-71.2716647093232,38.8885439073604,-427.99999999999));
#37238=CARTESIAN_POINT('Ctrl Pts',(-71.2711338421677,38.8884674414819,-428.009413591677));
#37239=CARTESIAN_POINT('',(-71.2680022706297,38.8994772862588,-427.99999999999));
#37240=CARTESIAN_POINT('Ctrl Pts',(-71.2680022706297,38.8994772862588,-427.99999999999));
#37241=CARTESIAN_POINT('Ctrl Pts',(-70.7169686230207,40.544463089243,-427.999999999993));
#37242=CARTESIAN_POINT('Ctrl Pts',(-69.9924483273869,42.1503621667178,-427.999999999994));
#37243=CARTESIAN_POINT('Ctrl Pts',(-68.2308187876938,45.1813402102631,-427.999999999994));
#37244=CARTESIAN_POINT('Ctrl Pts',(-67.1940828116546,46.6057769486988,-427.999999999994));
#37245=CARTESIAN_POINT('Ctrl Pts',(-66.0375105252203,47.8988186801189,-427.999999999992));
#37246=CARTESIAN_POINT('',(-71.7785821060461,47.3861904101294,-419.984638846405));
#37247=CARTESIAN_POINT('Ctrl Pts',(-71.7785821060662,47.3861904101271,-419.984638846386));
#37248=CARTESIAN_POINT('Ctrl Pts',(-71.7724611885407,47.2498667926128,-419.994305902311));
#37249=CARTESIAN_POINT('Ctrl Pts',(-71.7663232076033,47.113353314811,-420.004475138088));
#37250=CARTESIAN_POINT('Ctrl Pts',(-71.6665187924467,44.8971811433478,-420.178714023205));
#37251=CARTESIAN_POINT('Ctrl Pts',(-71.600564905539,43.4835729440167,-420.421072892069));
#37252=CARTESIAN_POINT('Ctrl Pts',(-71.5182713684043,41.8465706212519,-421.040387316386));
#37253=CARTESIAN_POINT('Ctrl Pts',(-71.4918599114317,41.3575832154767,-421.330101967646));
#37254=CARTESIAN_POINT('Ctrl Pts',(-71.443658195456,40.5515131717966,-422.07461693779));
#37255=CARTESIAN_POINT('Ctrl Pts',(-71.4213402659048,40.2265518059047,-422.539930138472));
#37256=CARTESIAN_POINT('Ctrl Pts',(-71.3770625254436,39.6877840871316,-423.727830620286));
#37257=CARTESIAN_POINT('Ctrl Pts',(-71.3545927816378,39.4679345708994,-424.464502550804));
#37258=CARTESIAN_POINT('Ctrl Pts',(-71.3080362258214,39.1148313554367,-426.246798891955));
#37259=CARTESIAN_POINT('Ctrl Pts',(-71.2860316626743,38.9892078161781,-427.192312295973));
#37260=CARTESIAN_POINT('Ctrl Pts',(-71.2680022706297,38.8994772862587,-427.99999999999));
#37261=CARTESIAN_POINT('Origin',(-64.400842226757,55.0197816364623,-409.61464763811));
#37262=CARTESIAN_POINT('Origin',(8.04911692853239E-13,-11.1690000000094,
-427.999999999986));
#37263=CARTESIAN_POINT('Origin',(47.765853049082,-53.3647801549723,-427.999999999982));
#37264=CARTESIAN_POINT('',(43.3329036555858,-83.6944436817575,-427.999999999976));
#37265=CARTESIAN_POINT('Origin',(42.1957801549698,-58.9348530490775,-427.99999999998));
#37266=CARTESIAN_POINT('',(-43.3329036555715,-83.6944436817652,-427.999999999975));
#37267=CARTESIAN_POINT('Origin',(-7.51898543427387E-11,859.831,-428.000000000083));
#37268=CARTESIAN_POINT('Origin',(-42.1957801549599,-58.9348530490849,-427.999999999979));
#37269=CARTESIAN_POINT('',(-72.5254436817472,-54.5019036555938,-427.999999999977));
#37270=CARTESIAN_POINT('Origin',(-47.7658530490669,-53.3647801549782,-427.99999999998));
#37271=CARTESIAN_POINT('',(-72.525443681755,32.1639036555634,-427.999999999987));
#37272=CARTESIAN_POINT('Origin',(871.,-11.1689999999327,-427.99999999999));
#37273=CARTESIAN_POINT('Origin',(-47.7658530490746,31.0267801549515,-427.99999999999));
#37274=CARTESIAN_POINT('',(-42.3714057377688,64.2789556966095,-427.999999999994));
#37275=CARTESIAN_POINT('Origin',(-34.2237874382673,30.734273111837,-427.99999999999));
#37276=CARTESIAN_POINT('',(42.3714057377573,64.278955696617,-427.999999999995));
#37277=CARTESIAN_POINT('Origin',(9.43689570931383E-12,-110.169000000009,
-427.999999999975));
#37278=CARTESIAN_POINT('Origin',(34.2237874382616,30.7342731118431,-427.999999999991));
#37279=CARTESIAN_POINT('Origin',(47.7658530490689,31.0267801549598,-427.999999999991));
#37280=CARTESIAN_POINT('Origin',(26.9899999999942,67.2000000000338,-73.7599999999943));
#37281=CARTESIAN_POINT('',(28.4333756729943,67.2000000000342,-71.2599999999944));
#37282=CARTESIAN_POINT('',(29.8767513458943,67.200000000034,-73.7599999999943));
#37283=CARTESIAN_POINT('',(29.1550635094443,67.2000000000341,-72.5099999999943));
#37284=CARTESIAN_POINT('',(28.4333756729943,67.2000000000336,-76.2599999999943));
#37285=CARTESIAN_POINT('',(29.1550635094443,67.2000000000338,-75.0099999999943));
#37286=CARTESIAN_POINT('',(25.5466243269943,67.2000000000334,-76.2599999999943));
#37287=CARTESIAN_POINT('',(26.9899999999942,67.2000000000335,-76.2599999999943));
#37288=CARTESIAN_POINT('',(24.1032486540943,67.2000000000335,-73.7599999999943));
#37289=CARTESIAN_POINT('',(24.8249364905443,67.2000000000334,-75.0099999999943));
#37290=CARTESIAN_POINT('',(25.5466243269943,67.2000000000339,-71.2599999999944));
#37291=CARTESIAN_POINT('',(24.8249364905443,67.2000000000337,-72.5099999999943));
#37292=CARTESIAN_POINT('',(27.7116878364943,67.2000000000341,-71.2599999999944));
#37293=CARTESIAN_POINT('Origin',(26.9999999999943,67.2000000000295,-110.759999999994));
#37294=CARTESIAN_POINT('',(28.4433756729943,67.2000000000299,-108.259999999994));
#37295=CARTESIAN_POINT('',(29.8867513458943,67.2000000000298,-110.759999999994));
#37296=CARTESIAN_POINT('',(29.1650635094443,67.2000000000299,-109.509999999994));
#37297=CARTESIAN_POINT('',(28.4433756729943,67.2000000000294,-113.259999999994));
#37298=CARTESIAN_POINT('',(29.1650635094443,67.2000000000295,-112.009999999994));
#37299=CARTESIAN_POINT('',(25.5566243269942,67.2000000000291,-113.259999999994));
#37300=CARTESIAN_POINT('',(26.9999999999943,67.2000000000292,-113.259999999994));
#37301=CARTESIAN_POINT('',(24.1132486540943,67.2000000000293,-110.759999999994));
#37302=CARTESIAN_POINT('',(24.8349364905443,67.2000000000291,-112.009999999994));
#37303=CARTESIAN_POINT('',(25.5566243269942,67.2000000000296,-108.259999999994));
#37304=CARTESIAN_POINT('',(24.8349364905443,67.2000000000295,-109.509999999994));
#37305=CARTESIAN_POINT('',(27.7216878364943,67.2000000000299,-108.259999999994));
#37306=CARTESIAN_POINT('Origin',(-55.0000000000061,71.331,-304.499999999995));
#37307=CARTESIAN_POINT('',(-1.50000000000603,70.3310000000047,-304.499999999994));
#37308=CARTESIAN_POINT('Origin',(50.9999999999939,71.3309999999974,-407.499999999995));
#37309=CARTESIAN_POINT('',(50.999999999994,70.3310000000034,-355.499999999994));
#37310=CARTESIAN_POINT('Origin',(-55.0000000000061,71.3309999999883,-406.499999999995));
#37311=CARTESIAN_POINT('',(-1.50000000000603,70.330999999993,-406.499999999995));
#37312=CARTESIAN_POINT('Origin',(-54.0000000000061,71.3309999999883,-407.499999999995));
#37313=CARTESIAN_POINT('',(-54.000000000006,70.3309999999942,-355.499999999994));
#37314=CARTESIAN_POINT('Origin',(-47.7658530490666,-53.3647801549749,-400.49999999998));
#37315=CARTESIAN_POINT('',(-73.0049525312943,-54.5239258606288,-400.499999999979));
#37316=CARTESIAN_POINT('',(-71.7514247672298,-61.3050642049046,-400.499999999979));
#37317=CARTESIAN_POINT('Origin',(-47.7658530490666,-53.3647801549749,-400.49999999998));
#37318=CARTESIAN_POINT('',(-73.0049525312945,-54.5239258606286,-400.499999999977));
#37319=CARTESIAN_POINT('Ctrl Pts',(-71.7514247672298,-61.3050642049046,
-400.499999999979));
#37320=CARTESIAN_POINT('Ctrl Pts',(-71.5902902839036,-61.2826808326117,
-409.666667134937));
#37321=CARTESIAN_POINT('Ctrl Pts',(-71.4291495149372,-61.2601533109042,
-418.833333808622));
#37322=CARTESIAN_POINT('Ctrl Pts',(-71.2680022706209,-61.2374772862897,
-427.999999999979));
#37323=CARTESIAN_POINT('Origin',(-72.1248916810212,-69.8588628384965,-400.499999999977));
#37324=CARTESIAN_POINT('',(-72.1248916810212,-69.8588628384965,-400.499999999977));
#37325=CARTESIAN_POINT('',(-72.1248916810212,-69.8588628384965,-400.499999999977));
#37326=CARTESIAN_POINT('',(-71.7514247672298,-61.3050642049048,-400.499999999978));
#37327=CARTESIAN_POINT('Origin',(-58.6898628384754,-83.2938916810397,-400.499999999976));
#37328=CARTESIAN_POINT('',(-58.6898628384754,-83.2938916810397,-400.499999999976));
#37329=CARTESIAN_POINT('',(-58.6898628384754,-83.2938916810397,-400.499999999976));
#37330=CARTESIAN_POINT('',(-72.1248916810212,-69.8588628384965,-400.499999999977));
#37331=CARTESIAN_POINT('Origin',(-50.136064204883,-82.9204247672467,-400.499999999976));
#37332=CARTESIAN_POINT('',(-50.1360642048832,-82.9204247672467,-400.499999999977));
#37333=CARTESIAN_POINT('Ctrl Pts',(-50.1360642048832,-82.9204247672467,
-400.499999999977));
#37334=CARTESIAN_POINT('Ctrl Pts',(-50.1136808325894,-82.7592902839214,
-409.666667134934));
#37335=CARTESIAN_POINT('Ctrl Pts',(-50.0911533108812,-82.5981495149561,
-418.83333380862));
#37336=CARTESIAN_POINT('Ctrl Pts',(-50.0684772862639,-82.4370022706413,
-427.999999999976));
#37337=CARTESIAN_POINT('',(-58.6898628384754,-83.2938916810397,-400.499999999976));
#37338=CARTESIAN_POINT('Origin',(-42.1957801549596,-58.9348530490817,-400.499999999979));
#37339=CARTESIAN_POINT('',(-43.3549258606093,-84.1739525313094,-400.499999999977));
#37340=CARTESIAN_POINT('Origin',(-42.1957801549596,-58.9348530490817,-400.49999999998));
#37341=CARTESIAN_POINT('',(-43.3549258606094,-84.1739525313095,-400.499999999977));
#37342=CARTESIAN_POINT('Origin',(-7.49122985865824E-11,859.831,-400.500000000088));
#37343=CARTESIAN_POINT('',(43.3549258606242,-84.1739525313017,-400.499999999978));
#37344=CARTESIAN_POINT('',(43.3549258606243,-84.1739525313017,-400.499999999977));
#37345=CARTESIAN_POINT('Origin',(-7.49122985865824E-11,859.831,-400.500000000087));
#37346=CARTESIAN_POINT('Origin',(42.1957801549702,-58.9348530490743,-400.499999999981));
#37347=CARTESIAN_POINT('',(50.1360642048978,-82.920424767238,-400.499999999978));
#37348=CARTESIAN_POINT('Origin',(42.1957801549702,-58.9348530490743,-400.499999999981));
#37349=CARTESIAN_POINT('Ctrl Pts',(50.1360642048978,-82.920424767238,-400.499999999978));
#37350=CARTESIAN_POINT('Ctrl Pts',(50.1136808326039,-82.7592902839127,-409.666667134936));
#37351=CARTESIAN_POINT('Ctrl Pts',(50.0911533108953,-82.5981495149473,-418.833333808621));
#37352=CARTESIAN_POINT('Ctrl Pts',(50.0684772862795,-82.4370022706321,-427.999999999977));
#37353=CARTESIAN_POINT('Origin',(50.1360642048978,-82.920424767238,-400.499999999978));
#37354=CARTESIAN_POINT('',(58.6898628384902,-83.2938916810294,-400.499999999977));
#37355=CARTESIAN_POINT('',(58.6898628384902,-83.2938916810295,-400.499999999978));
#37356=CARTESIAN_POINT('',(50.1360642048981,-82.920424767238,-400.499999999977));
#37357=CARTESIAN_POINT('Origin',(58.6898628384903,-83.2938916810294,-400.499999999978));
#37358=CARTESIAN_POINT('',(72.1248916810336,-69.8588628384839,-400.499999999979));
#37359=CARTESIAN_POINT('',(72.1248916810336,-69.8588628384839,-400.49999999998));
#37360=CARTESIAN_POINT('',(58.6898628384902,-83.2938916810294,-400.499999999977));
#37361=CARTESIAN_POINT('Origin',(72.1248916810336,-69.8588628384839,-400.49999999998));
#37362=CARTESIAN_POINT('',(71.7514247672407,-61.3050642048926,-400.499999999981));
#37363=CARTESIAN_POINT('Ctrl Pts',(71.7514247672407,-61.3050642048926,-400.499999999981));
#37364=CARTESIAN_POINT('Ctrl Pts',(71.5902902839144,-61.2826808325999,-409.666667134939));
#37365=CARTESIAN_POINT('Ctrl Pts',(71.4291495149477,-61.2601533108924,-418.833333808624));
#37366=CARTESIAN_POINT('Ctrl Pts',(71.2680022706319,-61.2374772862763,-427.999999999981));
#37367=CARTESIAN_POINT('',(72.1248916810336,-69.8588628384839,-400.499999999979));
#37368=CARTESIAN_POINT('Origin',(47.7658530490823,-53.3647801549691,-400.499999999981));
#37369=CARTESIAN_POINT('Origin',(47.7658530490823,-53.3647801549691,-400.499999999981));
#37370=CARTESIAN_POINT('Origin',(47.7658530490691,31.026780154963,-400.499999999991));
#37371=CARTESIAN_POINT('',(71.7491203026103,38.9740220215422,-400.499999999992));
#37372=CARTESIAN_POINT('Origin',(47.7658530490691,31.026780154963,-400.499999999991));
#37373=CARTESIAN_POINT('Ctrl Pts',(71.7491203026103,38.9740220215422,-400.499999999992));
#37374=CARTESIAN_POINT('Ctrl Pts',(71.5880199233528,38.9515086021118,-409.666667134328));
#37375=CARTESIAN_POINT('Ctrl Pts',(71.4269132622027,38.928852118611,-418.833333808083));
#37376=CARTESIAN_POINT('Ctrl Pts',(71.2658001171997,38.906048264694,-428.000000004049));
#37377=CARTESIAN_POINT('Origin',(72.1248916810234,47.5208628384841,-400.499999999993));
#37378=CARTESIAN_POINT('',(72.1248916810234,47.5208628384841,-400.499999999992));
#37379=CARTESIAN_POINT('',(72.1248916810234,47.5208628384841,-400.499999999993));
#37380=CARTESIAN_POINT('',(71.74912030261,38.9740220215367,-400.499999999992));
#37381=CARTESIAN_POINT('Origin',(58.6898628384777,60.9558916810272,-400.499999999994));
#37382=CARTESIAN_POINT('',(58.6898628384777,60.9558916810272,-400.499999999994));
#37383=CARTESIAN_POINT('',(58.6898628384777,60.9558916810272,-400.499999999994));
#37384=CARTESIAN_POINT('',(72.1248916810234,47.5208628384841,-400.499999999992));
#37385=CARTESIAN_POINT('Origin',(52.3435336415238,60.6788049642798,-400.499999999994));
#37386=CARTESIAN_POINT('',(52.3435287413493,60.6788047503336,-400.499999999994));
#37387=CARTESIAN_POINT('Ctrl Pts',(52.3435287413493,60.6788047503336,-400.499999999994));
#37388=CARTESIAN_POINT('Ctrl Pts',(52.3021261363478,60.5168398606716,-409.666667632972));
#37389=CARTESIAN_POINT('Ctrl Pts',(52.260542466553,60.3548670822409,-418.833334310633));
#37390=CARTESIAN_POINT('Ctrl Pts',(52.2187735884339,60.1928862347074,-427.999999999994));
#37391=CARTESIAN_POINT('',(58.6898628384777,60.9558916810272,-400.499999999994));
#37392=CARTESIAN_POINT('Origin',(34.2237874382619,30.7342731118462,-400.49999999999));
#37393=CARTESIAN_POINT('',(42.4847016472408,64.745407999866,-400.499999999994));
#37394=CARTESIAN_POINT('Origin',(34.2237874382619,30.7342731118462,-400.49999999999));
#37395=CARTESIAN_POINT('',(42.4847016472409,64.745407999866,-400.499999999994));
#37396=CARTESIAN_POINT('Origin',(9.74220704108575E-12,-110.169000000006,
-400.499999999973));
#37397=CARTESIAN_POINT('',(-42.4847016472518,64.7454079998587,-400.499999999984));
#37398=CARTESIAN_POINT('',(-42.4847016474569,64.7454080007027,-400.499999950222));
#37399=CARTESIAN_POINT('Origin',(9.74220704108575E-12,-110.169000000006,
-400.499999999973));
#37400=CARTESIAN_POINT('Origin',(-34.223787438267,30.7342731118402,-400.499999999974));
#37401=CARTESIAN_POINT('',(-52.3435287413598,60.6788047503246,-400.499999999984));
#37402=CARTESIAN_POINT('Origin',(-34.223787438267,30.7342731118402,-400.499999999974));
#37403=CARTESIAN_POINT('Ctrl Pts',(-52.3435287413598,60.6788047503246,-400.499999999984));
#37404=CARTESIAN_POINT('Ctrl Pts',(-52.3021261363584,60.5168398606624,-409.666667632968));
#37405=CARTESIAN_POINT('Ctrl Pts',(-52.2605424665637,60.3548670822318,-418.83333431063));
#37406=CARTESIAN_POINT('Ctrl Pts',(-52.2187735884448,60.1928862346983,-427.999999999992));
#37407=CARTESIAN_POINT('Origin',(-52.3435336415342,60.6788049642707,-400.499999999992));
#37408=CARTESIAN_POINT('',(-58.689862838488,60.955891681017,-400.499999999992));
#37409=CARTESIAN_POINT('',(-58.689862838488,60.955891681017,-400.499999999992));
#37410=CARTESIAN_POINT('',(-52.3435287413607,60.6788047503247,-400.499999999992));
#37411=CARTESIAN_POINT('Origin',(-58.689862838488,60.955891681017,-400.499999999992));
#37412=CARTESIAN_POINT('',(-72.1248916810314,47.5208628384715,-400.499999999991));
#37413=CARTESIAN_POINT('',(-72.1248916810314,47.5208628384715,-400.499999999991));
#37414=CARTESIAN_POINT('',(-58.689862838488,60.955891681017,-400.499999999992));
#37415=CARTESIAN_POINT('Origin',(-72.1248916810314,47.5208628384715,-400.499999999991));
#37416=CARTESIAN_POINT('',(-71.7514247672385,38.96706420488,-400.49999999999));
#37417=CARTESIAN_POINT('Ctrl Pts',(-71.7514247672385,38.96706420488,-400.49999999999));
#37418=CARTESIAN_POINT('Ctrl Pts',(-71.5902902839124,38.944680832585,-409.666667134948));
#37419=CARTESIAN_POINT('Ctrl Pts',(-71.4291495149459,38.9221533108755,-418.833333808634));
#37420=CARTESIAN_POINT('Ctrl Pts',(-71.2680022706297,38.8994772862588,-427.99999999999));
#37421=CARTESIAN_POINT('',(-72.1248916810314,47.5208628384715,-400.499999999991));
#37422=CARTESIAN_POINT('Origin',(-47.7658530490743,31.0267801549546,-400.49999999999));
#37423=CARTESIAN_POINT('',(-73.004952531302,32.1859258606045,-400.499999999989));
#37424=CARTESIAN_POINT('Origin',(-47.7658530490743,31.0267801549546,-400.49999999999));
#37425=CARTESIAN_POINT('',(-73.0049525313019,32.1859258606049,-400.499999999988));
#37426=CARTESIAN_POINT('Origin',(871.,-11.1689999999296,-400.499999999992));
#37427=CARTESIAN_POINT('Origin',(871.,-11.1689999999296,-400.499999999994));
#37428=CARTESIAN_POINT('Origin',(27.7116878364939,71.2000000000341,-71.2599999999948));
#37429=CARTESIAN_POINT('',(28.4333756729939,71.0000000000342,-71.2599999999948));
#37430=CARTESIAN_POINT('',(28.4333756729939,71.2000000000342,-71.2599999999948));
#37431=CARTESIAN_POINT('',(25.5466243269939,71.0000000000339,-71.2599999999948));
#37432=CARTESIAN_POINT('',(25.5466243269939,71.2000000000339,-71.2599999999948));
#37433=CARTESIAN_POINT('',(26.9899999999939,71.0000000000341,-71.2599999999948));
#37434=CARTESIAN_POINT('Origin',(24.8249364905439,71.2000000000337,-72.5099999999948));
#37435=CARTESIAN_POINT('',(24.1032486540939,71.0000000000336,-73.7599999999948));
#37436=CARTESIAN_POINT('',(24.1032486540939,71.2000000000335,-73.7599999999948));
#37437=CARTESIAN_POINT('',(25.5466243269939,71.0000000000339,-71.2599999999948));
#37438=CARTESIAN_POINT('Origin',(24.8249364905439,71.2000000000334,-75.0099999999948));
#37439=CARTESIAN_POINT('',(25.5466243269939,71.0000000000333,-76.2599999999948));
#37440=CARTESIAN_POINT('',(25.5466243269939,71.2000000000333,-76.2599999999948));
#37441=CARTESIAN_POINT('',(24.1032486540939,71.0000000000336,-73.7599999999948));
#37442=CARTESIAN_POINT('Origin',(26.9899999999939,71.2000000000334,-76.2599999999948));
#37443=CARTESIAN_POINT('',(28.4333756729939,71.0000000000336,-76.2599999999948));
#37444=CARTESIAN_POINT('',(28.4333756729939,71.2000000000336,-76.2599999999948));
#37445=CARTESIAN_POINT('',(26.9899999999939,71.0000000000334,-76.2599999999948));
#37446=CARTESIAN_POINT('Origin',(29.1550635094439,71.2000000000338,-75.0099999999948));
#37447=CARTESIAN_POINT('',(29.876751345894,71.0000000000341,-73.7599999999948));
#37448=CARTESIAN_POINT('',(29.8767513458939,71.200000000034,-73.7599999999948));
#37449=CARTESIAN_POINT('',(28.4333756729939,71.0000000000336,-76.2599999999948));
#37450=CARTESIAN_POINT('Origin',(29.1550635094439,71.2000000000341,-72.5099999999948));
#37451=CARTESIAN_POINT('',(29.876751345894,71.0000000000341,-73.7599999999948));
#37452=CARTESIAN_POINT('Origin',(27.7216878364939,71.2000000000299,-108.259999999995));
#37453=CARTESIAN_POINT('',(28.443375672994,71.0000000000299,-108.259999999995));
#37454=CARTESIAN_POINT('',(28.4433756729939,71.2000000000299,-108.259999999995));
#37455=CARTESIAN_POINT('',(25.5566243269939,71.0000000000297,-108.259999999995));
#37456=CARTESIAN_POINT('',(25.5566243269939,71.2000000000296,-108.259999999995));
#37457=CARTESIAN_POINT('',(26.9999999999939,71.0000000000298,-108.259999999995));
#37458=CARTESIAN_POINT('Origin',(24.8349364905439,71.2000000000295,-109.509999999995));
#37459=CARTESIAN_POINT('',(24.1132486540939,71.0000000000293,-110.759999999995));
#37460=CARTESIAN_POINT('',(24.1132486540939,71.2000000000293,-110.759999999995));
#37461=CARTESIAN_POINT('',(25.5566243269939,71.0000000000297,-108.259999999995));
#37462=CARTESIAN_POINT('Origin',(24.8349364905439,71.2000000000291,-112.009999999995));
#37463=CARTESIAN_POINT('',(25.5566243269939,71.0000000000291,-113.259999999995));
#37464=CARTESIAN_POINT('',(25.5566243269939,71.2000000000291,-113.259999999995));
#37465=CARTESIAN_POINT('',(24.1132486540939,71.0000000000293,-110.759999999995));
#37466=CARTESIAN_POINT('Origin',(26.9999999999939,71.2000000000292,-113.259999999995));
#37467=CARTESIAN_POINT('',(28.443375672994,71.0000000000294,-113.259999999995));
#37468=CARTESIAN_POINT('',(28.4433756729939,71.2000000000294,-113.259999999995));
#37469=CARTESIAN_POINT('',(26.9999999999939,71.0000000000292,-113.259999999995));
#37470=CARTESIAN_POINT('Origin',(29.165063509444,71.2000000000295,-112.009999999995));
#37471=CARTESIAN_POINT('',(29.8867513458939,71.0000000000298,-110.759999999995));
#37472=CARTESIAN_POINT('',(29.8867513458939,71.2000000000298,-110.759999999995));
#37473=CARTESIAN_POINT('',(28.443375672994,71.0000000000294,-113.259999999995));
#37474=CARTESIAN_POINT('Origin',(29.165063509444,71.2000000000299,-109.509999999995));
#37475=CARTESIAN_POINT('',(29.8867513458939,71.0000000000298,-110.759999999995));
#37476=CARTESIAN_POINT('Origin',(1.11022302462516E-12,-11.1690000000053,
-392.499999999986));
#37477=CARTESIAN_POINT('',(59.7537315194951,21.2885348647401,-400.499999999989));
#37478=CARTESIAN_POINT('',(59.7537315195008,-43.6265348647421,-400.499999999981));
#37479=CARTESIAN_POINT('Origin',(1.11022302462516E-12,-11.1690000000062,
-400.499999999986));
#37480=CARTESIAN_POINT('',(59.7537315194951,21.2885348647406,-395.499999999989));
#37481=CARTESIAN_POINT('',(59.7537315194951,21.288534864741,-392.499999999989));
#37482=CARTESIAN_POINT('',(59.7537315195008,-43.6265348647416,-395.499999999981));
#37483=CARTESIAN_POINT('Origin',(1.11022302462516E-12,-11.1690000000057,
-395.499999999985));
#37484=CARTESIAN_POINT('',(59.7537315195008,-43.6265348647412,-392.499999999982));
#37485=CARTESIAN_POINT('Origin',(1.11022302462516E-12,-11.1690000000053,
-392.499999999986));
#37486=CARTESIAN_POINT('',(50.0390320947648,47.355313469007,-392.499999999992));
#37487=CARTESIAN_POINT('',(58.524313469004,38.8700320947692,-392.499999999991));
#37488=CARTESIAN_POINT('Origin',(1.11022302462516E-12,-11.1690000000053,
-392.499999999986));
#37489=CARTESIAN_POINT('',(58.524313469004,38.8700320947683,-400.499999999991));
#37490=CARTESIAN_POINT('',(58.524313469004,38.8700320947692,-392.499999999991));
#37491=CARTESIAN_POINT('',(50.0390320947648,47.3553134690061,-400.499999999992));
#37492=CARTESIAN_POINT('Origin',(1.11022302462516E-12,-11.1690000000062,
-400.499999999986));
#37493=CARTESIAN_POINT('',(50.0390320947648,47.355313469007,-392.499999999992));
#37494=CARTESIAN_POINT('Origin',(-1.50000000000603,70.3309999999988,-355.499999999994));
#37495=CARTESIAN_POINT('',(42.499999999994,70.3310000000076,-312.999999999994));
#37496=CARTESIAN_POINT('',(42.499999999994,70.3309999999978,-397.999999999994));
#37497=CARTESIAN_POINT('',(42.499999999994,70.3310000000076,-312.999999999994));
#37498=CARTESIAN_POINT('',(-42.5000000000061,70.3309999999903,-397.999999999994));
#37499=CARTESIAN_POINT('',(42.499999999994,70.3309999999978,-397.999999999994));
#37500=CARTESIAN_POINT('',(-42.5000000000061,70.331,-312.999999999995));
#37501=CARTESIAN_POINT('',(-42.5000000000061,70.331,-312.999999999994));
#37502=CARTESIAN_POINT('',(42.499999999994,70.3310000000076,-312.999999999994));
#37503=CARTESIAN_POINT('Origin',(42.499999999994,70.3309999999978,-397.999999999994));
#37504=CARTESIAN_POINT('',(32.4575348647363,48.5847315194942,-397.999999999992));
#37505=CARTESIAN_POINT('',(42.4999999999959,47.8824939485326,-397.999999999992));
#37506=CARTESIAN_POINT('',(32.4575348647364,48.5847315194942,-397.999999999992));
#37507=CARTESIAN_POINT('',(-32.4575348647446,48.5847315194885,-397.999999999992));
#37508=CARTESIAN_POINT('Origin',(1.11022302462516E-12,-11.1690000000059,
-397.999999999985));
#37509=CARTESIAN_POINT('',(-42.5000000000041,47.8824939485251,-397.999999999992));
#37510=CARTESIAN_POINT('',(-50.0390320947728,47.3553134689976,-397.999999999992));
#37511=CARTESIAN_POINT('',(-42.5000000000061,70.3309999999903,-397.999999999994));
#37512=CARTESIAN_POINT('',(42.499999999994,70.3309999999978,-397.999999999994));
#37513=CARTESIAN_POINT('Origin',(1.11022302462516E-12,-11.1690000000053,
-392.499999999986));
#37514=CARTESIAN_POINT('',(-32.4575348647446,48.5847315194882,-400.499999999992));
#37515=CARTESIAN_POINT('',(-32.4575348647446,48.5847315194891,-392.499999999992));
#37516=CARTESIAN_POINT('',(32.4575348647363,48.5847315194939,-400.499999999992));
#37517=CARTESIAN_POINT('',(32.4575348647364,48.5847315194948,-392.499999999992));
#37518=CARTESIAN_POINT('Origin',(1.11022302462516E-12,-11.1690000000062,
-400.499999999986));
#37519=CARTESIAN_POINT('Origin',(1.11022302462516E-12,-11.1690000000053,
-392.499999999986));
#37520=CARTESIAN_POINT('',(-58.5243134690106,38.8700320947589,-392.499999999991));
#37521=CARTESIAN_POINT('',(-50.0390320947728,47.3553134689982,-392.499999999992));
#37522=CARTESIAN_POINT('Origin',(1.11022302462516E-12,-11.1690000000053,
-392.499999999986));
#37523=CARTESIAN_POINT('',(-50.0390320947728,47.3553134689973,-400.499999999992));
#37524=CARTESIAN_POINT('',(-50.0390320947728,47.3553134689982,-392.499999999992));
#37525=CARTESIAN_POINT('',(-58.5243134690106,38.8700320947581,-400.499999999991));
#37526=CARTESIAN_POINT('Origin',(1.11022302462516E-12,-11.1690000000062,
-400.499999999986));
#37527=CARTESIAN_POINT('',(-58.5243134690106,38.870032094759,-392.499999999991));
#37528=CARTESIAN_POINT('Origin',(1.11022302462516E-12,-11.1690000000053,
-392.499999999986));
#37529=CARTESIAN_POINT('',(-59.753731519493,-43.6265348647525,-400.499999999981));
#37530=CARTESIAN_POINT('',(-59.7537315194986,21.2885348647297,-400.499999999989));
#37531=CARTESIAN_POINT('Origin',(1.11022302462516E-12,-11.1690000000062,
-400.499999999986));
#37532=CARTESIAN_POINT('',(-59.753731519493,-43.626534864752,-395.499999999981));
#37533=CARTESIAN_POINT('',(-59.753731519493,-43.6265348647516,-392.499999999982));
#37534=CARTESIAN_POINT('',(-59.7537315194986,21.2885348647302,-395.499999999989));
#37535=CARTESIAN_POINT('Origin',(1.11022302462516E-12,-11.1690000000057,
-395.499999999985));
#37536=CARTESIAN_POINT('',(-59.7537315194986,21.2885348647306,-392.499999999989));
#37537=CARTESIAN_POINT('Origin',(1.11022302462516E-12,-11.1690000000053,
-392.499999999986));
#37538=CARTESIAN_POINT('',(-50.0390320947626,-69.6933134690176,-392.499999999978));
#37539=CARTESIAN_POINT('',(-58.5243134690019,-61.2080320947798,-392.49999999998));
#37540=CARTESIAN_POINT('Origin',(1.11022302462516E-12,-11.1690000000053,
-392.499999999986));
#37541=CARTESIAN_POINT('',(-58.5243134690019,-61.2080320947807,-400.49999999998));
#37542=CARTESIAN_POINT('',(-58.5243134690019,-61.2080320947798,-392.49999999998));
#37543=CARTESIAN_POINT('',(-50.0390320947626,-69.6933134690185,-400.499999999979));
#37544=CARTESIAN_POINT('Origin',(1.11022302462516E-12,-11.1690000000062,
-400.499999999986));
#37545=CARTESIAN_POINT('',(-50.0390320947626,-69.6933134690176,-392.499999999978));
#37546=CARTESIAN_POINT('Origin',(-47.7658530490666,-53.3647801549749,-400.49999999998));
#37547=CARTESIAN_POINT('',(-58.5243134690019,-61.2080320947808,-400.49999999998));
#37548=CARTESIAN_POINT('',(-59.7537315194986,21.2885348647297,-400.499999999989));
#37549=CARTESIAN_POINT('',(-50.0390320947728,47.3553134689973,-400.499999999992));
#37550=CARTESIAN_POINT('',(32.4575348647364,48.5847315194939,-400.499999999992));
#37551=CARTESIAN_POINT('',(58.524313469004,38.8700320947682,-400.499999999991));
#37552=CARTESIAN_POINT('',(58.5243134690129,-61.2080320947705,-400.49999999998));
#37553=CARTESIAN_POINT('',(59.7537315195008,-43.6265348647421,-400.499999999981));
#37554=CARTESIAN_POINT('',(50.039032094775,-69.6933134690098,-400.499999999979));
#37555=CARTESIAN_POINT('Origin',(1.11022302462516E-12,-11.1690000000062,
-400.499999999986));
#37556=CARTESIAN_POINT('',(50.039032094775,-69.6933134690098,-400.499999999979));
#37557=CARTESIAN_POINT('',(-32.4575348647342,-70.9227315195064,-400.499999999979));
#37558=CARTESIAN_POINT('Origin',(1.11022302462516E-12,-11.1690000000053,
-392.499999999986));
#37559=CARTESIAN_POINT('',(58.5243134690129,-61.2080320947695,-392.49999999998));
#37560=CARTESIAN_POINT('',(50.039032094775,-69.6933134690089,-392.499999999978));
#37561=CARTESIAN_POINT('Origin',(1.11022302462516E-12,-11.1690000000053,
-392.499999999986));
#37562=CARTESIAN_POINT('',(50.039032094775,-69.6933134690089,-392.499999999978));
#37563=CARTESIAN_POINT('',(58.5243134690129,-61.2080320947695,-392.49999999998));
#37564=CARTESIAN_POINT('Origin',(26.9899999999939,71.0000000000338,-73.7599999999948));
#37565=CARTESIAN_POINT('Origin',(26.9999999999939,71.0000000000295,-110.759999999995));
#37566=CARTESIAN_POINT('Origin',(59.7537315195008,-43.6265348647412,-392.499999999982));
#37567=CARTESIAN_POINT('',(58.8129254661913,-57.0806882454319,-395.49999999998));
#37568=CARTESIAN_POINT('',(59.7537315195008,-43.6265348647416,-395.499999999981));
#37569=CARTESIAN_POINT('',(58.8129254661914,-57.0806882454316,-392.49999999998));
#37570=CARTESIAN_POINT('',(58.8129254661913,-57.0806882454319,-395.49999999998));
#37571=CARTESIAN_POINT('',(58.8129254661914,-57.0806882454316,-392.49999999998));
#37572=CARTESIAN_POINT('Origin',(58.524313469004,38.8700320947692,-392.499999999991));
#37573=CARTESIAN_POINT('',(58.8129254661833,34.7426882454313,-392.49999999999));
#37574=CARTESIAN_POINT('',(58.524313469004,38.8700320947692,-392.499999999991));
#37575=CARTESIAN_POINT('',(58.8129254661833,34.7426882454309,-395.49999999999));
#37576=CARTESIAN_POINT('',(58.8129254661833,34.7426882454309,-395.49999999999));
#37577=CARTESIAN_POINT('',(58.8129254661833,34.742688245431,-395.49999999999));
#37578=CARTESIAN_POINT('Origin',(-41.9116882454246,-76.0623577133481,-395.499999999978));
#37579=CARTESIAN_POINT('',(64.8933577133359,34.7426882454314,-395.49999999999));
#37580=CARTESIAN_POINT('',(50.9116882454285,34.7426882454302,-395.49999999999));
#37581=CARTESIAN_POINT('',(68.6020931316032,32.2411146190954,-395.49999999999));
#37582=CARTESIAN_POINT('Origin',(64.8933577133362,30.7426882454314,-395.49999999999));
#37583=CARTESIAN_POINT('',(71.999999999998,23.8310000000006,-395.49999999999));
#37584=CARTESIAN_POINT('',(68.6020931316032,32.2411146190954,-395.49999999999));
#37585=CARTESIAN_POINT('',(72.0000000000041,-46.1689999999994,-395.499999999981));
#37586=CARTESIAN_POINT('',(72.0000000000041,-46.1689999999994,-395.499999999981));
#37587=CARTESIAN_POINT('',(68.6020931316108,-54.5791146190948,-395.499999999981));
#37588=CARTESIAN_POINT('',(68.6020931316108,-54.5791146190948,-395.499999999981));
#37589=CARTESIAN_POINT('',(64.8933577133439,-57.0806882454314,-395.49999999998));
#37590=CARTESIAN_POINT('Origin',(64.8933577133436,-53.0806882454314,-395.499999999981));
#37591=CARTESIAN_POINT('',(50.9116882454365,-57.0806882454326,-395.49999999998));
#37592=CARTESIAN_POINT('Origin',(50.9116882454281,39.7426882454302,-395.499999999991));
#37593=CARTESIAN_POINT('',(45.9116882454281,39.7426882454301,-392.499999999991));
#37594=CARTESIAN_POINT('',(45.9116882454281,39.7426882454482,-235.499999999991));
#37595=CARTESIAN_POINT('',(45.9116882454281,39.7426882454298,-395.499999999991));
#37596=CARTESIAN_POINT('',(50.9116882454285,34.7426882454486,-235.499999999991));
#37597=CARTESIAN_POINT('Origin',(50.9116882454281,39.7426882454486,-235.499999999991));
#37598=CARTESIAN_POINT('',(50.9116882454285,34.7426882454305,-392.49999999999));
#37599=CARTESIAN_POINT('',(50.9116882454285,34.7426882454302,-395.49999999999));
#37600=CARTESIAN_POINT('Origin',(50.9116882454281,39.7426882454305,-392.499999999991));
#37601=CARTESIAN_POINT('Origin',(32.4575348647364,48.5847315194948,-392.499999999992));
#37602=CARTESIAN_POINT('',(42.4999999999959,47.8824939485329,-395.499999999992));
#37603=CARTESIAN_POINT('',(42.4999999999959,47.8824939485424,-312.999999999992));
#37604=CARTESIAN_POINT('',(45.9116882454274,47.6439254661849,-395.499999999992));
#37605=CARTESIAN_POINT('',(42.4999999999959,47.8824939485329,-395.499999999992));
#37606=CARTESIAN_POINT('',(45.9116882454274,47.6439254661853,-392.499999999992));
#37607=CARTESIAN_POINT('',(45.9116882454274,47.6439254661849,-395.499999999992));
#37608=CARTESIAN_POINT('',(45.9116882454274,47.6439254661854,-392.499999999992));
#37609=CARTESIAN_POINT('Origin',(1.11022302462516E-12,-11.1690000000053,
-392.499999999986));
#37610=CARTESIAN_POINT('',(45.9116882454281,39.7426882454301,-392.499999999991));
#37611=CARTESIAN_POINT('',(50.9116882454285,34.7426882454305,-392.49999999999));
#37612=CARTESIAN_POINT('Origin',(-41.9116882454246,-76.0623577133481,-395.499999999978));
#37613=CARTESIAN_POINT('',(43.4101146190902,57.4330931316041,-395.499999999993));
#37614=CARTESIAN_POINT('',(42.4999999999951,57.8008033062343,-395.499999999993));
#37615=CARTESIAN_POINT('',(43.4101146190903,57.433093131604,-395.499999999993));
#37616=CARTESIAN_POINT('',(45.9116882454268,53.7243577133371,-395.499999999993));
#37617=CARTESIAN_POINT('Origin',(41.9116882454268,53.7243577133368,-395.499999999993));
#37618=CARTESIAN_POINT('',(45.9116882454281,39.7426882454298,-395.499999999991));
#37619=CARTESIAN_POINT('',(42.499999999994,70.3309999999981,-395.499999999994));
#37620=CARTESIAN_POINT('Origin',(42.499999999994,70.3310000000076,-312.999999999994));
#37621=CARTESIAN_POINT('',(42.4999999999951,57.8008033062439,-312.999999999993));
#37622=CARTESIAN_POINT('',(42.4999999999951,57.8008033062344,-395.499999999993));
#37623=CARTESIAN_POINT('',(42.499999999994,70.3310000000076,-312.999999999994));
#37624=CARTESIAN_POINT('Origin',(-42.5000000000061,70.331,-312.999999999994));
#37625=CARTESIAN_POINT('',(-42.500000000005,57.8008033062269,-395.499999999993));
#37626=CARTESIAN_POINT('',(-42.500000000005,57.8008033062364,-312.999999999993));
#37627=CARTESIAN_POINT('',(-42.500000000005,57.800803306227,-395.499999999993));
#37628=CARTESIAN_POINT('',(-42.5000000000061,70.331,-312.999999999995));
#37629=CARTESIAN_POINT('',(-42.5000000000041,47.8824939485254,-395.499999999992));
#37630=CARTESIAN_POINT('',(-42.5000000000041,47.8824939485258,-392.499999999992));
#37631=CARTESIAN_POINT('',(-42.4999999999932,-76.0623577133482,-395.499999999978));
#37632=CARTESIAN_POINT('Origin',(42.499999999994,70.3310000000076,-312.999999999994));
#37633=CARTESIAN_POINT('',(-35.0000000000052,60.8310000000008,-312.999999999993));
#37634=CARTESIAN_POINT('',(-43.4101146191,57.433093131606,-312.999999999993));
#37635=CARTESIAN_POINT('',(34.9999999999948,60.8310000000069,-312.999999999993));
#37636=CARTESIAN_POINT('',(34.9999999999948,60.8310000000069,-312.999999999993));
#37637=CARTESIAN_POINT('',(43.4101146190902,57.4330931316135,-312.999999999993));
#37638=CARTESIAN_POINT('Origin',(-50.0390320947728,47.3553134689982,-392.499999999992));
#37639=CARTESIAN_POINT('',(-45.9116882454354,47.6439254661774,-392.499999999992));
#37640=CARTESIAN_POINT('',(-45.9116882454354,47.643925466177,-395.499999999992));
#37641=CARTESIAN_POINT('',(-45.9116882454354,47.6439254661771,-395.499999999992));
#37642=CARTESIAN_POINT('',(-45.9116882454354,47.643925466177,-395.499999999992));
#37643=CARTESIAN_POINT('',(-50.0390320947728,47.3553134689982,-392.499999999992));
#37644=CARTESIAN_POINT('Origin',(-41.9116882454246,-76.0623577133481,-395.499999999978));
#37645=CARTESIAN_POINT('',(-45.911688245436,53.7243577133291,-395.499999999993));
#37646=CARTESIAN_POINT('',(-45.9116882454348,39.7426882454218,-395.499999999991));
#37647=CARTESIAN_POINT('',(-43.4101146191,57.4330931315965,-395.499999999993));
#37648=CARTESIAN_POINT('Origin',(-41.911688245436,53.7243577133295,-395.499999999993));
#37649=CARTESIAN_POINT('',(-43.4101146191,57.4330931315965,-395.499999999993));
#37650=CARTESIAN_POINT('Origin',(-50.9116882454347,39.7426882454213,-395.499999999991));
#37651=CARTESIAN_POINT('',(-50.9116882454343,34.7426882454217,-392.49999999999));
#37652=CARTESIAN_POINT('',(-50.9116882454343,34.7426882454398,-235.499999999991));
#37653=CARTESIAN_POINT('',(-50.9116882454343,34.7426882454213,-395.49999999999));
#37654=CARTESIAN_POINT('',(-45.9116882454348,39.7426882454402,-235.499999999991));
#37655=CARTESIAN_POINT('Origin',(-50.9116882454347,39.7426882454398,-235.499999999991));
#37656=CARTESIAN_POINT('',(-45.9116882454348,39.7426882454221,-392.499999999991));
#37657=CARTESIAN_POINT('',(-45.9116882454348,39.7426882454218,-395.499999999991));
#37658=CARTESIAN_POINT('Origin',(-50.9116882454347,39.7426882454217,-392.499999999991));
#37659=CARTESIAN_POINT('Origin',(-59.7537315194986,21.2885348647306,-392.499999999989));
#37660=CARTESIAN_POINT('',(-58.8129254661891,34.7426882454206,-395.49999999999));
#37661=CARTESIAN_POINT('',(-59.7537315194986,21.2885348647302,-395.499999999989));
#37662=CARTESIAN_POINT('',(-58.8129254661891,34.742688245421,-392.49999999999));
#37663=CARTESIAN_POINT('',(-58.8129254661891,34.7426882454206,-395.49999999999));
#37664=CARTESIAN_POINT('',(-58.8129254661891,34.742688245421,-392.49999999999));
#37665=CARTESIAN_POINT('Origin',(1.11022302462516E-12,-11.1690000000053,
-392.499999999986));
#37666=CARTESIAN_POINT('',(-50.9116882454343,34.7426882454217,-392.49999999999));
#37667=CARTESIAN_POINT('',(-45.9116882454348,39.7426882454221,-392.499999999991));
#37668=CARTESIAN_POINT('Origin',(-58.5243134690019,-61.2080320947798,-392.49999999998));
#37669=CARTESIAN_POINT('',(-58.8129254661811,-57.0806882454418,-392.49999999998));
#37670=CARTESIAN_POINT('',(-58.5243134690019,-61.2080320947798,-392.49999999998));
#37671=CARTESIAN_POINT('',(-58.8129254661811,-57.0806882454422,-395.49999999998));
#37672=CARTESIAN_POINT('',(-58.8129254661811,-57.0806882454422,-395.49999999998));
#37673=CARTESIAN_POINT('',(-58.8129254661811,-57.0806882454422,-395.49999999998));
#37674=CARTESIAN_POINT('Origin',(-41.9116882454246,-76.0623577133481,-395.499999999978));
#37675=CARTESIAN_POINT('',(-64.8933577133337,-57.0806882454427,-395.49999999998));
#37676=CARTESIAN_POINT('',(-50.9116882454263,-57.0806882454415,-395.49999999998));
#37677=CARTESIAN_POINT('',(-68.602093131601,-54.5791146191067,-395.499999999981));
#37678=CARTESIAN_POINT('Origin',(-64.893357713334,-53.0806882454427,-395.499999999981));
#37679=CARTESIAN_POINT('',(-71.9999999999959,-46.1690000000119,-395.499999999981));
#37680=CARTESIAN_POINT('',(-68.602093131601,-54.5791146191067,-395.499999999981));
#37681=CARTESIAN_POINT('',(-72.000000000002,23.8309999999881,-395.49999999999));
#37682=CARTESIAN_POINT('',(-72.000000000002,23.8309999999881,-395.49999999999));
#37683=CARTESIAN_POINT('',(-68.6020931316086,32.2411146190835,-395.49999999999));
#37684=CARTESIAN_POINT('',(-68.6020931316086,32.2411146190835,-395.49999999999));
#37685=CARTESIAN_POINT('',(-64.8933577133417,34.7426882454201,-395.49999999999));
#37686=CARTESIAN_POINT('Origin',(-64.8933577133413,30.7426882454201,-395.49999999999));
#37687=CARTESIAN_POINT('',(-50.9116882454343,34.7426882454213,-395.49999999999));
#37688=CARTESIAN_POINT('Origin',(-50.9116882454259,-62.0806882454415,-395.49999999998));
#37689=CARTESIAN_POINT('',(-45.9116882454259,-62.0806882454407,-392.49999999998));
#37690=CARTESIAN_POINT('',(-45.9116882454259,-62.0806882454226,-235.49999999998));
#37691=CARTESIAN_POINT('',(-45.9116882454259,-62.0806882454411,-395.49999999998));
#37692=CARTESIAN_POINT('',(-50.9116882454263,-57.0806882454231,-235.49999999998));
#37693=CARTESIAN_POINT('Origin',(-50.9116882454259,-62.0806882454231,-235.49999999998));
#37694=CARTESIAN_POINT('',(-50.9116882454263,-57.0806882454411,-392.49999999998));
#37695=CARTESIAN_POINT('',(-50.9116882454263,-57.0806882454415,-395.49999999998));
#37696=CARTESIAN_POINT('Origin',(-50.9116882454259,-62.0806882454412,-392.49999999998));
#37697=CARTESIAN_POINT('Origin',(-32.4575348647342,-70.9227315195055,-392.499999999978));
#37698=CARTESIAN_POINT('',(-45.9116882454252,-69.9819254661964,-395.499999999979));
#37699=CARTESIAN_POINT('',(-32.4575348647341,-70.9227315195058,-395.499999999979));
#37700=CARTESIAN_POINT('',(-45.9116882454252,-69.981925466196,-392.499999999978));
#37701=CARTESIAN_POINT('',(-45.9116882454252,-69.9819254661964,-395.499999999979));
#37702=CARTESIAN_POINT('',(-45.9116882454252,-69.981925466196,-392.499999999978));
#37703=CARTESIAN_POINT('Origin',(1.11022302462516E-12,-11.1690000000053,
-392.499999999986));
#37704=CARTESIAN_POINT('',(-45.9116882454259,-62.0806882454407,-392.49999999998));
#37705=CARTESIAN_POINT('',(-50.9116882454263,-57.0806882454411,-392.49999999998));
#37706=CARTESIAN_POINT('Origin',(50.9116882454369,-62.0806882454326,-395.49999999998));
#37707=CARTESIAN_POINT('',(50.9116882454365,-57.0806882454323,-392.49999999998));
#37708=CARTESIAN_POINT('',(50.9116882454365,-57.0806882454142,-235.49999999998));
#37709=CARTESIAN_POINT('',(50.9116882454365,-57.0806882454326,-395.49999999998));
#37710=CARTESIAN_POINT('',(45.9116882454369,-62.0806882454146,-235.49999999998));
#37711=CARTESIAN_POINT('Origin',(50.9116882454369,-62.0806882454142,-235.49999999998));
#37712=CARTESIAN_POINT('',(45.9116882454369,-62.0806882454327,-392.49999999998));
#37713=CARTESIAN_POINT('',(45.9116882454369,-62.0806882454331,-395.49999999998));
#37714=CARTESIAN_POINT('Origin',(50.9116882454369,-62.0806882454323,-392.49999999998));
#37715=CARTESIAN_POINT('Origin',(1.11022302462516E-12,-11.1690000000053,
-392.499999999986));
#37716=CARTESIAN_POINT('',(50.9116882454365,-57.0806882454323,-392.49999999998));
#37717=CARTESIAN_POINT('',(45.9116882454377,-69.981925466188,-392.499999999978));
#37718=CARTESIAN_POINT('',(45.9116882454369,-62.0806882454327,-392.49999999998));
#37719=CARTESIAN_POINT('',(50.039032094775,-69.6933134690089,-392.499999999978));
#37720=CARTESIAN_POINT('Origin',(50.039032094775,-69.6933134690089,-392.499999999978));
#37721=CARTESIAN_POINT('',(45.9116882454377,-69.9819254661884,-395.499999999979));
#37722=CARTESIAN_POINT('',(45.9116882454377,-69.9819254661884,-395.499999999979));
#37723=CARTESIAN_POINT('',(45.9116882454377,-69.9819254661884,-395.499999999979));
#37724=CARTESIAN_POINT('Origin',(-41.9116882454246,-76.0623577133481,-395.499999999978));
#37725=CARTESIAN_POINT('',(45.9116882454382,-76.0623577133405,-395.499999999978));
#37726=CARTESIAN_POINT('',(45.9116882454369,-62.0806882454331,-395.49999999998));
#37727=CARTESIAN_POINT('',(43.4101146191022,-79.7710931316078,-395.499999999977));
#37728=CARTESIAN_POINT('Origin',(41.9116882454381,-76.0623577133408,-395.499999999978));
#37729=CARTESIAN_POINT('',(35.0000000000074,-83.1690000000026,-395.499999999977));
#37730=CARTESIAN_POINT('',(43.4101146191022,-79.7710931316078,-395.499999999977));
#37731=CARTESIAN_POINT('',(-34.9999999999926,-83.1690000000087,-395.499999999977));
#37732=CARTESIAN_POINT('',(-34.9999999999926,-83.1690000000087,-395.499999999977));
#37733=CARTESIAN_POINT('',(-43.410114619088,-79.7710931316154,-395.499999999977));
#37734=CARTESIAN_POINT('',(-43.4101146190881,-79.7710931316153,-395.499999999977));
#37735=CARTESIAN_POINT('',(-45.9116882454247,-76.0623577133485,-395.499999999978));
#37736=CARTESIAN_POINT('Origin',(-41.9116882454246,-76.0623577133481,-395.499999999978));
#37737=CARTESIAN_POINT('',(-45.9116882454259,-62.0806882454411,-395.49999999998));
#37738=CARTESIAN_POINT('Origin',(-58.8178305978845,-25.7906133403662,-211.686857166486));
#37739=CARTESIAN_POINT('',(-59.591244465674,-33.9502909241456,-201.14447126204));
#37740=CARTESIAN_POINT('',(-59.1711016649654,-32.5796982421243,-203.651996219616));
#37741=CARTESIAN_POINT('',(-59.5912444656741,-33.9502909241456,-201.14447126204));
#37742=CARTESIAN_POINT('',(-57.7748829601655,-33.9034515013528,-205.804258601751));
#37743=CARTESIAN_POINT('',(-59.1711016649654,-32.5796982421241,-203.651996219616));
#37744=CARTESIAN_POINT('',(-56.7988070560068,-36.5977974427891,-205.448996026285));
#37745=CARTESIAN_POINT('',(-57.7748829601653,-33.9034515013528,-205.804258601751));
#37746=CARTESIAN_POINT('',(-57.2189498567156,-37.9683901248104,-202.941471068708));
#37747=CARTESIAN_POINT('',(-56.7988070560068,-36.5977974427891,-205.448996026285));
#37748=CARTESIAN_POINT('',(-58.6151685615154,-36.6446368655819,-200.789208686573));
#37749=CARTESIAN_POINT('',(-57.2189498567156,-37.9683901248105,-202.941471068708));
#37750=CARTESIAN_POINT('',(-58.6151685615154,-36.6446368655819,-200.789208686573));
#37751=CARTESIAN_POINT('Origin',(-1.720845688169E-12,21.037500000044,35.000000000011));
#37752=CARTESIAN_POINT('',(3.96999999999828,21.037500000041,7.00000000001097));
#37753=CARTESIAN_POINT('',(-3.97000000000172,21.0375000000404,7.00000000001097));
#37754=CARTESIAN_POINT('',(-1.720845688169E-12,21.0375000000407,7.00000000001097));
#37755=CARTESIAN_POINT('',(-3.97000000000172,21.0375000000469,63.0000000000109));
#37756=CARTESIAN_POINT('',(-3.97000000000172,21.0375000000436,35.000000000011));
#37757=CARTESIAN_POINT('',(3.96999999999828,21.0375000000475,63.0000000000109));
#37758=CARTESIAN_POINT('',(-1.720845688169E-12,21.0375000000472,63.0000000000109));
#37759=CARTESIAN_POINT('',(3.96999999999828,21.0375000000443,35.000000000011));
#37760=CARTESIAN_POINT('Origin',(8.32667268468867E-13,-8.23124999995205,
70.0000000000143));
#37761=CARTESIAN_POINT('Origin',(1.11022302462516E-12,-11.1689999999872,
-235.499999999986));
#37762=CARTESIAN_POINT('',(50.039032094775,-69.6933134689908,-235.499999999979));
#37763=CARTESIAN_POINT('',(45.9116882454377,-69.9819254661699,-235.499999999979));
#37764=CARTESIAN_POINT('',(50.039032094775,-69.6933134689908,-235.499999999979));
#37765=CARTESIAN_POINT('',(45.9116882454369,-62.0806882454146,-235.49999999998));
#37766=CARTESIAN_POINT('',(58.8129254661914,-57.0806882454135,-235.49999999998));
#37767=CARTESIAN_POINT('',(50.9116882454365,-57.0806882454142,-235.49999999998));
#37768=CARTESIAN_POINT('',(58.5243134690129,-61.2080320947514,-235.49999999998));
#37769=CARTESIAN_POINT('',(58.5243134690129,-61.2080320947515,-235.49999999998));
#37770=CARTESIAN_POINT('Origin',(1.11022302462516E-12,-11.1689999999872,
-235.499999999986));
#37771=CARTESIAN_POINT('Origin',(1.11022302462516E-12,-11.1689999999872,
-235.499999999986));
#37772=CARTESIAN_POINT('',(58.5243134690129,-61.2080320947505,-227.49999999998));
#37773=CARTESIAN_POINT('',(58.5243134690129,-61.2080320947514,-235.49999999998));
#37774=CARTESIAN_POINT('',(50.039032094775,-69.6933134689899,-227.499999999979));
#37775=CARTESIAN_POINT('Origin',(1.11022302462516E-12,-11.1689999999863,
-227.499999999986));
#37776=CARTESIAN_POINT('',(50.039032094775,-69.6933134689908,-235.499999999979));
#37777=CARTESIAN_POINT('Origin',(50.9116882454365,-57.0806882454326,-395.49999999998));
#37778=CARTESIAN_POINT('',(64.8933577133439,-57.0806882454126,-232.49999999998));
#37779=CARTESIAN_POINT('',(64.8933577133439,-57.0806882454314,-395.49999999998));
#37780=CARTESIAN_POINT('',(58.8129254661914,-57.0806882454131,-232.49999999998));
#37781=CARTESIAN_POINT('',(-41.9116882454263,-57.0806882454219,-232.49999999998));
#37782=CARTESIAN_POINT('',(58.8129254661914,-57.0806882454135,-235.49999999998));
#37783=CARTESIAN_POINT('Origin',(64.8933577133436,-53.0806882454314,-395.499999999981));
#37784=CARTESIAN_POINT('',(68.6020931316108,-54.579114619076,-232.499999999981));
#37785=CARTESIAN_POINT('',(68.6020931316108,-54.5791146190948,-395.499999999981));
#37786=CARTESIAN_POINT('Origin',(64.8933577133436,-53.0806882454126,-232.499999999981));
#37787=CARTESIAN_POINT('Origin',(68.6020931316108,-54.5791146190948,-395.499999999981));
#37788=CARTESIAN_POINT('',(72.0000000000041,-46.1689999999806,-232.499999999982));
#37789=CARTESIAN_POINT('',(72.0000000000041,-46.1689999999994,-395.499999999981));
#37790=CARTESIAN_POINT('',(68.6020931316108,-54.579114619076,-232.499999999981));
#37791=CARTESIAN_POINT('Origin',(72.0000000000041,-46.1689999999994,-395.499999999981));
#37792=CARTESIAN_POINT('',(71.999999999998,23.8310000000193,-232.49999999999));
#37793=CARTESIAN_POINT('',(71.999999999998,23.8310000000006,-395.49999999999));
#37794=CARTESIAN_POINT('',(72.0000000000068,-76.0623577133194,-232.499999999978));
#37795=CARTESIAN_POINT('Origin',(68.6020931316032,32.2411146190954,-395.49999999999));
#37796=CARTESIAN_POINT('',(68.6020931316032,32.2411146191142,-232.499999999991));
#37797=CARTESIAN_POINT('',(68.6020931316032,32.2411146190954,-395.49999999999));
#37798=CARTESIAN_POINT('',(71.999999999998,23.8310000000194,-232.49999999999));
#37799=CARTESIAN_POINT('Origin',(64.8933577133362,30.7426882454314,-395.49999999999));
#37800=CARTESIAN_POINT('',(64.8933577133359,34.7426882454502,-232.499999999991));
#37801=CARTESIAN_POINT('',(64.8933577133359,34.7426882454314,-395.49999999999));
#37802=CARTESIAN_POINT('Origin',(64.8933577133362,30.7426882454502,-232.49999999999));
#37803=CARTESIAN_POINT('Origin',(50.9116882454285,34.7426882454302,-395.49999999999));
#37804=CARTESIAN_POINT('',(58.8129254661834,34.7426882454493,-235.499999999991));
#37805=CARTESIAN_POINT('',(-2.91433543964104E-12,34.7426882454442,-235.499999999991));
#37806=CARTESIAN_POINT('',(58.8129254661834,34.7426882454497,-232.499999999991));
#37807=CARTESIAN_POINT('',(58.8129254661834,34.7426882454493,-235.499999999991));
#37808=CARTESIAN_POINT('',(-41.9116882454343,34.7426882454409,-232.499999999991));
#37809=CARTESIAN_POINT('Origin',(1.11022302462516E-12,-11.1689999999872,
-235.499999999986));
#37810=CARTESIAN_POINT('',(58.5243134690041,38.8700320947872,-235.499999999991));
#37811=CARTESIAN_POINT('',(58.5243134690041,38.8700320947873,-235.499999999991));
#37812=CARTESIAN_POINT('',(45.9116882454274,47.6439254662035,-235.499999999992));
#37813=CARTESIAN_POINT('',(45.9116882454281,39.7426882454482,-235.499999999991));
#37814=CARTESIAN_POINT('',(50.0390320947648,47.355313469025,-235.499999999992));
#37815=CARTESIAN_POINT('',(50.0390320947648,47.355313469025,-235.499999999992));
#37816=CARTESIAN_POINT('Origin',(1.11022302462516E-12,-11.1689999999872,
-235.499999999986));
#37817=CARTESIAN_POINT('Origin',(1.11022302462516E-12,-11.1689999999872,
-235.499999999986));
#37818=CARTESIAN_POINT('',(50.0390320947648,47.355313469026,-227.499999999992));
#37819=CARTESIAN_POINT('',(50.0390320947648,47.355313469025,-235.499999999992));
#37820=CARTESIAN_POINT('',(58.5243134690041,38.8700320947882,-227.499999999991));
#37821=CARTESIAN_POINT('Origin',(1.11022302462516E-12,-11.1689999999863,
-227.499999999986));
#37822=CARTESIAN_POINT('',(58.5243134690041,38.8700320947873,-235.499999999991));
#37823=CARTESIAN_POINT('Origin',(45.9116882454281,39.7426882454298,-395.499999999991));
#37824=CARTESIAN_POINT('',(45.9116882454268,53.7243577133559,-232.499999999993));
#37825=CARTESIAN_POINT('',(45.9116882454268,53.7243577133371,-395.499999999993));
#37826=CARTESIAN_POINT('',(45.9116882454274,47.6439254662038,-232.499999999992));
#37827=CARTESIAN_POINT('',(45.9116882454382,-76.0623577133217,-232.499999999978));
#37828=CARTESIAN_POINT('',(45.9116882454274,47.6439254662035,-235.499999999992));
#37829=CARTESIAN_POINT('Origin',(41.9116882454268,53.7243577133368,-395.499999999993));
#37830=CARTESIAN_POINT('',(43.4101146190902,57.4330931316228,-232.499999999993));
#37831=CARTESIAN_POINT('',(43.4101146190902,57.433093131604,-395.499999999993));
#37832=CARTESIAN_POINT('Origin',(41.9116882454268,53.7243577133556,-232.499999999993));
#37833=CARTESIAN_POINT('Origin',(43.4101146190902,57.433093131604,-395.499999999993));
#37834=CARTESIAN_POINT('',(34.9999999999948,60.8310000000162,-232.499999999994));
#37835=CARTESIAN_POINT('',(34.9999999999948,60.8309999999974,-395.499999999994));
#37836=CARTESIAN_POINT('',(43.4101146190903,57.4330931316228,-232.499999999993));
#37837=CARTESIAN_POINT('Origin',(34.9999999999948,60.8309999999974,-395.499999999994));
#37838=CARTESIAN_POINT('',(-35.0000000000052,60.8310000000101,-232.499999999994));
#37839=CARTESIAN_POINT('',(-35.0000000000052,60.8309999999913,-395.499999999994));
#37840=CARTESIAN_POINT('',(-41.9116882454366,60.8310000000095,-232.499999999994));
#37841=CARTESIAN_POINT('Origin',(-43.4101146191,57.4330931315965,-395.499999999993));
#37842=CARTESIAN_POINT('',(-43.4101146191,57.4330931316153,-232.499999999993));
#37843=CARTESIAN_POINT('',(-43.4101146191,57.4330931315965,-395.499999999993));
#37844=CARTESIAN_POINT('',(-35.0000000000052,60.8310000000101,-232.499999999994));
#37845=CARTESIAN_POINT('Origin',(-41.911688245436,53.7243577133295,-395.499999999993));
#37846=CARTESIAN_POINT('',(-45.911688245436,53.7243577133479,-232.499999999993));
#37847=CARTESIAN_POINT('',(-45.911688245436,53.7243577133291,-395.499999999993));
#37848=CARTESIAN_POINT('Origin',(-41.911688245436,53.7243577133483,-232.499999999993));
#37849=CARTESIAN_POINT('Origin',(-45.9116882454348,39.7426882454218,-395.499999999991));
#37850=CARTESIAN_POINT('',(-45.9116882454354,47.6439254661955,-235.499999999992));
#37851=CARTESIAN_POINT('',(-45.9116882454303,-11.1689999999912,-235.499999999986));
#37852=CARTESIAN_POINT('',(-45.9116882454354,47.6439254661958,-232.499999999992));
#37853=CARTESIAN_POINT('',(-45.9116882454354,47.6439254661955,-235.499999999992));
#37854=CARTESIAN_POINT('',(-45.9116882454247,-76.0623577133297,-232.499999999978));
#37855=CARTESIAN_POINT('Origin',(1.11022302462516E-12,-11.1689999999872,
-235.499999999986));
#37856=CARTESIAN_POINT('',(-50.0390320947728,47.3553134690163,-235.499999999992));
#37857=CARTESIAN_POINT('',(-50.0390320947728,47.3553134690163,-235.499999999992));
#37858=CARTESIAN_POINT('',(-58.8129254661892,34.7426882454391,-235.499999999991));
#37859=CARTESIAN_POINT('',(-50.9116882454343,34.7426882454398,-235.499999999991));
#37860=CARTESIAN_POINT('',(-58.5243134690107,38.870032094777,-235.499999999991));
#37861=CARTESIAN_POINT('',(-58.5243134690107,38.870032094777,-235.499999999991));
#37862=CARTESIAN_POINT('Origin',(1.11022302462516E-12,-11.1689999999872,
-235.499999999986));
#37863=CARTESIAN_POINT('Origin',(1.11022302462516E-12,-11.1689999999872,
-235.499999999986));
#37864=CARTESIAN_POINT('',(-58.5243134690107,38.870032094778,-227.499999999991));
#37865=CARTESIAN_POINT('',(-58.5243134690107,38.870032094777,-235.499999999991));
#37866=CARTESIAN_POINT('',(-50.0390320947728,47.3553134690172,-227.499999999992));
#37867=CARTESIAN_POINT('Origin',(1.11022302462516E-12,-11.1689999999863,
-227.499999999986));
#37868=CARTESIAN_POINT('',(-50.0390320947728,47.3553134690163,-235.499999999992));
#37869=CARTESIAN_POINT('Origin',(-50.9116882454343,34.7426882454213,-395.49999999999));
#37870=CARTESIAN_POINT('',(-64.8933577133417,34.7426882454388,-232.499999999991));
#37871=CARTESIAN_POINT('',(-64.8933577133417,34.7426882454201,-395.49999999999));
#37872=CARTESIAN_POINT('',(-58.8129254661891,34.7426882454394,-232.499999999991));
#37873=CARTESIAN_POINT('',(-41.9116882454343,34.7426882454409,-232.499999999991));
#37874=CARTESIAN_POINT('',(-58.8129254661892,34.7426882454391,-235.499999999991));
#37875=CARTESIAN_POINT('Origin',(-64.8933577133413,30.7426882454201,-395.49999999999));
#37876=CARTESIAN_POINT('',(-68.6020931316086,32.2411146191022,-232.499999999991));
#37877=CARTESIAN_POINT('',(-68.6020931316086,32.2411146190835,-395.49999999999));
#37878=CARTESIAN_POINT('Origin',(-64.8933577133413,30.7426882454389,-232.49999999999));
#37879=CARTESIAN_POINT('Origin',(-68.6020931316086,32.2411146190835,-395.49999999999));
#37880=CARTESIAN_POINT('',(-72.000000000002,23.8310000000068,-232.49999999999));
#37881=CARTESIAN_POINT('',(-72.000000000002,23.8309999999881,-395.49999999999));
#37882=CARTESIAN_POINT('',(-68.6020931316086,32.2411146191022,-232.499999999991));
#37883=CARTESIAN_POINT('Origin',(-72.000000000002,23.8309999999881,-395.49999999999));
#37884=CARTESIAN_POINT('',(-71.9999999999959,-46.1689999999932,-232.499999999982));
#37885=CARTESIAN_POINT('',(-71.9999999999959,-46.1690000000119,-395.499999999981));
#37886=CARTESIAN_POINT('',(-71.9999999999933,-76.062357713332,-232.499999999978));
#37887=CARTESIAN_POINT('Origin',(-68.602093131601,-54.5791146191067,-395.499999999981));
#37888=CARTESIAN_POINT('',(-68.602093131601,-54.579114619088,-232.499999999981));
#37889=CARTESIAN_POINT('',(-68.602093131601,-54.5791146191068,-395.499999999981));
#37890=CARTESIAN_POINT('',(-71.9999999999959,-46.1689999999932,-232.499999999982));
#37891=CARTESIAN_POINT('Origin',(-64.893357713334,-53.0806882454427,-395.499999999981));
#37892=CARTESIAN_POINT('',(-64.8933577133337,-57.0806882454239,-232.49999999998));
#37893=CARTESIAN_POINT('',(-64.8933577133337,-57.0806882454427,-395.49999999998));
#37894=CARTESIAN_POINT('Origin',(-64.893357713334,-53.0806882454239,-232.499999999981));
#37895=CARTESIAN_POINT('Origin',(-50.9116882454263,-57.0806882454415,-395.49999999998));
#37896=CARTESIAN_POINT('',(-58.8129254661811,-57.0806882454238,-235.49999999998));
#37897=CARTESIAN_POINT('',(5.10702591327572E-12,-57.0806882454186,-235.49999999998));
#37898=CARTESIAN_POINT('',(-58.8129254661811,-57.0806882454234,-232.49999999998));
#37899=CARTESIAN_POINT('',(-58.8129254661812,-57.0806882454238,-235.49999999998));
#37900=CARTESIAN_POINT('',(-41.9116882454263,-57.0806882454219,-232.49999999998));
#37901=CARTESIAN_POINT('Origin',(1.11022302462516E-12,-11.1689999999872,
-235.499999999986));
#37902=CARTESIAN_POINT('',(-58.5243134690019,-61.2080320947617,-235.49999999998));
#37903=CARTESIAN_POINT('',(-58.5243134690019,-61.2080320947617,-235.49999999998));
#37904=CARTESIAN_POINT('',(-45.9116882454252,-69.9819254661779,-235.499999999979));
#37905=CARTESIAN_POINT('',(-45.9116882454259,-62.0806882454226,-235.49999999998));
#37906=CARTESIAN_POINT('',(-50.0390320947626,-69.6933134689995,-235.499999999979));
#37907=CARTESIAN_POINT('',(-50.0390320947626,-69.6933134689995,-235.499999999979));
#37908=CARTESIAN_POINT('Origin',(1.11022302462516E-12,-11.1689999999872,
-235.499999999986));
#37909=CARTESIAN_POINT('Origin',(1.11022302462516E-12,-11.1689999999872,
-235.499999999986));
#37910=CARTESIAN_POINT('',(-50.0390320947626,-69.6933134689986,-227.499999999979));
#37911=CARTESIAN_POINT('',(-50.0390320947626,-69.6933134689995,-235.499999999979));
#37912=CARTESIAN_POINT('',(-58.5243134690019,-61.2080320947608,-227.49999999998));
#37913=CARTESIAN_POINT('Origin',(1.11022302462516E-12,-11.1689999999863,
-227.499999999986));
#37914=CARTESIAN_POINT('',(-58.5243134690019,-61.2080320947617,-235.49999999998));
#37915=CARTESIAN_POINT('Origin',(-45.9116882454259,-62.0806882454411,-395.49999999998));
#37916=CARTESIAN_POINT('',(-45.9116882454246,-76.0623577133297,-232.499999999978));
#37917=CARTESIAN_POINT('',(-45.9116882454246,-76.0623577133485,-395.499999999978));
#37918=CARTESIAN_POINT('',(-45.9116882454252,-69.9819254661776,-232.499999999979));
#37919=CARTESIAN_POINT('',(-45.9116882454247,-76.0623577133297,-232.499999999978));
#37920=CARTESIAN_POINT('',(-45.9116882454252,-69.9819254661779,-235.499999999979));
#37921=CARTESIAN_POINT('Origin',(-41.9116882454246,-76.0623577133481,-395.499999999978));
#37922=CARTESIAN_POINT('',(-43.410114619088,-79.7710931315966,-232.499999999978));
#37923=CARTESIAN_POINT('',(-43.4101146190881,-79.7710931316153,-395.499999999977));
#37924=CARTESIAN_POINT('Origin',(-41.9116882454246,-76.0623577133294,-232.499999999978));
#37925=CARTESIAN_POINT('Origin',(-43.4101146190881,-79.7710931316153,-395.499999999977));
#37926=CARTESIAN_POINT('',(-34.9999999999926,-83.1689999999899,-232.499999999977));
#37927=CARTESIAN_POINT('',(-34.9999999999926,-83.1690000000087,-395.499999999977));
#37928=CARTESIAN_POINT('',(-43.4101146190881,-79.7710931315966,-232.499999999978));
#37929=CARTESIAN_POINT('Origin',(-34.9999999999926,-83.1690000000087,-395.499999999977));
#37930=CARTESIAN_POINT('',(35.0000000000075,-83.1689999999838,-232.499999999977));
#37931=CARTESIAN_POINT('',(35.0000000000074,-83.1690000000026,-395.499999999977));
#37932=CARTESIAN_POINT('',(-41.911688245424,-83.1689999999905,-232.499999999977));
#37933=CARTESIAN_POINT('Origin',(43.4101146191022,-79.7710931316078,-395.499999999977));
#37934=CARTESIAN_POINT('',(43.4101146191022,-79.771093131589,-232.499999999978));
#37935=CARTESIAN_POINT('',(43.4101146191022,-79.7710931316078,-395.499999999977));
#37936=CARTESIAN_POINT('',(35.0000000000074,-83.1689999999838,-232.499999999977));
#37937=CARTESIAN_POINT('Origin',(41.9116882454381,-76.0623577133408,-395.499999999978));
#37938=CARTESIAN_POINT('',(45.9116882454382,-76.0623577133217,-232.499999999978));
#37939=CARTESIAN_POINT('',(45.9116882454382,-76.0623577133405,-395.499999999978));
#37940=CARTESIAN_POINT('Origin',(41.9116882454381,-76.062357713322,-232.499999999978));
#37941=CARTESIAN_POINT('Origin',(45.9116882454369,-62.0806882454331,-395.49999999998));
#37942=CARTESIAN_POINT('',(45.9116882454377,-69.9819254661696,-232.499999999979));
#37943=CARTESIAN_POINT('',(45.9116882454377,-69.9819254661699,-235.499999999979));
#37944=CARTESIAN_POINT('',(45.9116882454382,-76.0623577133217,-232.499999999978));
#37945=CARTESIAN_POINT('Origin',(-62.7912238833522,-36.1419811084888,-202.309168520235));
#37946=CARTESIAN_POINT('',(-62.0126566584211,-38.1422389714875,-202.02579322501));
#37947=CARTESIAN_POINT('',(-58.6151685615155,-36.644636865582,-200.789208686573));
#37948=CARTESIAN_POINT('',(-63.0507462916694,-35.4752284874923,-202.403626951979));
#37949=CARTESIAN_POINT('',(-63.0507462916927,-35.4752284875026,-202.403626951987));
#37950=CARTESIAN_POINT('',(-63.0507462916617,-35.4752284874888,-202.403626951975));
#37951=CARTESIAN_POINT('Origin',(-61.3256090710095,-38.8089915924427,-203.10595056927));
#37952=CARTESIAN_POINT('',(-60.6385614835859,-39.4757442133925,-204.186107913527));
#37953=CARTESIAN_POINT('',(-57.2189498567157,-37.9683901248103,-202.941471068708));
#37954=CARTESIAN_POINT('',(-62.0126566584124,-38.1422389714836,-202.025793225006));
#37955=CARTESIAN_POINT('Origin',(-60.4705587127634,-38.8089915924429,-205.45518212126));
#37956=CARTESIAN_POINT('',(-60.3025559419268,-38.1422389714871,-206.724256328988));
#37957=CARTESIAN_POINT('',(-56.7988070560067,-36.5977974427891,-205.448996026285));
#37958=CARTESIAN_POINT('',(-60.6385614835583,-39.4757442133804,-204.186107913517));
#37959=CARTESIAN_POINT('Origin',(-60.8216007585505,-36.8087337294892,-206.913173192472));
#37960=CARTESIAN_POINT('',(-61.3406455751751,-35.4752284874919,-207.102090055957));
#37961=CARTESIAN_POINT('',(-57.7748829601656,-33.9034515013526,-205.804258601751));
#37962=CARTESIAN_POINT('',(-60.3025559419125,-38.1422389714808,-206.724256328982));
#37963=CARTESIAN_POINT('Origin',(-62.0276931625839,-34.8084758665355,-206.021932711695));
#37964=CARTESIAN_POINT('',(-62.7147407500105,-34.1417232455869,-204.941775367439));
#37965=CARTESIAN_POINT('',(-59.1711016649653,-32.5796982421245,-203.651996219616));
#37966=CARTESIAN_POINT('',(-61.3406455751928,-35.4752284874997,-207.102090055963));
#37967=CARTESIAN_POINT('Origin',(-62.8827435208299,-34.8084758665353,-203.672701159705));
#37968=CARTESIAN_POINT('',(-62.7147407500469,-34.141723245603,-204.941775367452));
#37969=CARTESIAN_POINT('Origin',(26.9899999999942,67.0000000000338,-73.7599999999943));
#37970=CARTESIAN_POINT('Origin',(26.9999999999943,67.0000000000297,-110.759999999994));
#37971=CARTESIAN_POINT('Origin',(-3.9700000000008,10.5187500000436,35.0000000000122));
#37972=CARTESIAN_POINT('',(-3.9700000000008,10.5187500000468,63.0000000000122));
#37973=CARTESIAN_POINT('',(-3.9700000000008,10.5187500000404,7.00000000001219));
#37974=CARTESIAN_POINT('Origin',(-8.04911692853239E-13,10.5187500000407,
7.00000000001219));
#37975=CARTESIAN_POINT('',(3.96999999999919,10.518750000041,7.00000000001219));
#37976=CARTESIAN_POINT('Origin',(3.96999999999919,10.5187500000443,35.0000000000122));
#37977=CARTESIAN_POINT('',(3.96999999999919,10.5187500000475,63.0000000000122));
#37978=CARTESIAN_POINT('Origin',(-8.04911692853239E-13,10.5187500000472,
63.0000000000122));
#37979=CARTESIAN_POINT('Origin',(-64.9999999999989,-11.1689999999867,-181.499999999986));
#37980=CARTESIAN_POINT('Origin',(-4.57966997657877E-12,53.831000000019,
-181.499999999993));
#37981=CARTESIAN_POINT('Origin',(65.0000000000011,-11.1689999999753,-181.499999999986));
#37982=CARTESIAN_POINT('Origin',(6.77236045021346E-12,-76.168999999981,
-181.499999999978));
#37983=CARTESIAN_POINT('Origin',(50.039032094775,-69.6933134689908,-235.499999999979));
#37984=CARTESIAN_POINT('',(32.4575348647468,-70.9227315194807,-227.499999999979));
#37985=CARTESIAN_POINT('',(50.039032094775,-69.6933134689898,-227.499999999979));
#37986=CARTESIAN_POINT('',(32.4575348647468,-70.9227315194813,-232.499999999979));
#37987=CARTESIAN_POINT('',(32.4575348647468,-70.9227315194816,-235.499999999979));
#37988=CARTESIAN_POINT('',(45.9116882454377,-69.9819254661696,-232.499999999979));
#37989=CARTESIAN_POINT('Origin',(1.11022302462516E-12,-11.1689999999863,
-227.499999999986));
#37990=CARTESIAN_POINT('',(58.1696747238672,-60.8533933496047,-227.49999999998));
#37991=CARTESIAN_POINT('',(59.3192302506027,-44.413983418182,-227.499999999982));
#37992=CARTESIAN_POINT('',(59.3192302506027,-44.4139834181821,-227.499999999982));
#37993=CARTESIAN_POINT('',(49.6843933496294,-69.338674723844,-227.499999999979));
#37994=CARTESIAN_POINT('Origin',(1.11022302462516E-12,-11.1689999999863,
-227.499999999986));
#37995=CARTESIAN_POINT('',(33.2449834182068,-70.4882302505823,-227.499999999979));
#37996=CARTESIAN_POINT('',(33.2449834182068,-70.4882302505823,-227.499999999979));
#37997=CARTESIAN_POINT('Origin',(1.11022302462516E-12,-11.1689999999863,
-227.499999999986));
#37998=CARTESIAN_POINT('',(59.7537315195009,-43.6265348647221,-227.499999999982));
#37999=CARTESIAN_POINT('',(58.5243134690129,-61.2080320947506,-227.49999999998));
#38000=CARTESIAN_POINT('Origin',(1.11022302462516E-12,-11.1689999999863,
-227.499999999986));
#38001=CARTESIAN_POINT('Origin',(58.5243134690129,-61.2080320947515,-235.49999999998));
#38002=CARTESIAN_POINT('',(59.7537315195008,-43.6265348647228,-232.499999999982));
#38003=CARTESIAN_POINT('',(59.7537315195008,-43.6265348647228,-232.499999999982));
#38004=CARTESIAN_POINT('',(59.7537315195008,-43.6265348647231,-235.499999999981));
#38005=CARTESIAN_POINT('Origin',(-41.9116882454246,-76.0623577133294,-232.499999999978));
#38006=CARTESIAN_POINT('',(59.7537315194952,21.2885348647593,-232.499999999989));
#38007=CARTESIAN_POINT('',(58.5243134690041,38.8700320947876,-232.499999999991));
#38008=CARTESIAN_POINT('Origin',(1.11022302462516E-12,-11.1689999999869,
-232.499999999986));
#38009=CARTESIAN_POINT('Origin',(58.5243134690041,38.8700320947873,-235.499999999991));
#38010=CARTESIAN_POINT('',(59.7537315194952,21.2885348647599,-227.499999999989));
#38011=CARTESIAN_POINT('',(58.5243134690041,38.8700320947882,-227.499999999991));
#38012=CARTESIAN_POINT('',(59.7537315194952,21.2885348647591,-235.499999999989));
#38013=CARTESIAN_POINT('Origin',(1.11022302462516E-12,-11.1689999999863,
-227.499999999986));
#38014=CARTESIAN_POINT('',(49.6843933496193,47.0006747238801,-227.499999999992));
#38015=CARTESIAN_POINT('',(33.2449834181965,48.1502302506155,-227.499999999992));
#38016=CARTESIAN_POINT('',(58.1696747238586,38.5153933496423,-227.499999999991));
#38017=CARTESIAN_POINT('Origin',(1.11022302462516E-12,-11.1689999999863,
-227.499999999986));
#38018=CARTESIAN_POINT('',(59.3192302505969,22.0759834182197,-227.499999999989));
#38019=CARTESIAN_POINT('',(59.3192302505969,22.0759834182197,-227.499999999989));
#38020=CARTESIAN_POINT('Origin',(1.11022302462516E-12,-11.1689999999863,
-227.499999999986));
#38021=CARTESIAN_POINT('',(50.0390320947648,47.355313469026,-227.499999999992));
#38022=CARTESIAN_POINT('Origin',(50.0390320947648,47.355313469025,-235.499999999992));
#38023=CARTESIAN_POINT('',(32.4575348647364,48.5847315195132,-232.499999999992));
#38024=CARTESIAN_POINT('Origin',(-41.9116882454246,-76.0623577133294,-232.499999999978));
#38025=CARTESIAN_POINT('',(-50.0390320947728,47.3553134690167,-232.499999999992));
#38026=CARTESIAN_POINT('Origin',(-50.0390320947728,47.3553134690163,-235.499999999992));
#38027=CARTESIAN_POINT('',(-50.0390320947728,47.3553134690172,-227.499999999992));
#38028=CARTESIAN_POINT('Origin',(1.11022302462516E-12,-11.1689999999863,
-227.499999999986));
#38029=CARTESIAN_POINT('',(-59.7537315194987,21.2885348647495,-227.499999999989));
#38030=CARTESIAN_POINT('',(-58.5243134690107,38.870032094778,-227.499999999991));
#38031=CARTESIAN_POINT('',(-59.3192302506006,22.0759834182094,-227.499999999989));
#38032=CARTESIAN_POINT('Origin',(1.11022302462516E-12,-11.1689999999863,
-227.499999999986));
#38033=CARTESIAN_POINT('',(-58.169674723865,38.5153933496321,-227.499999999991));
#38034=CARTESIAN_POINT('',(-59.3192302506005,22.0759834182094,-227.499999999989));
#38035=CARTESIAN_POINT('',(-49.6843933496272,47.0006747238714,-227.499999999992));
#38036=CARTESIAN_POINT('Origin',(1.11022302462516E-12,-11.1689999999863,
-227.499999999986));
#38037=CARTESIAN_POINT('',(-33.2449834182046,48.1502302506097,-227.499999999992));
#38038=CARTESIAN_POINT('Origin',(-58.5243134690107,38.870032094777,-235.499999999991));
#38039=CARTESIAN_POINT('',(-59.7537315194986,21.288534864749,-232.499999999989));
#38040=CARTESIAN_POINT('',(-59.7537315194986,21.288534864749,-232.499999999989));
#38041=CARTESIAN_POINT('',(-59.7537315194986,21.2885348647486,-235.499999999989));
#38042=CARTESIAN_POINT('Origin',(-41.9116882454246,-76.0623577133294,-232.499999999978));
#38043=CARTESIAN_POINT('',(-59.753731519493,-43.6265348647331,-232.499999999982));
#38044=CARTESIAN_POINT('',(-58.5243134690019,-61.2080320947614,-232.49999999998));
#38045=CARTESIAN_POINT('Origin',(1.11022302462516E-12,-11.1689999999869,
-232.499999999986));
#38046=CARTESIAN_POINT('Origin',(-58.5243134690019,-61.2080320947617,-235.49999999998));
#38047=CARTESIAN_POINT('',(-59.753731519493,-43.6265348647326,-227.499999999982));
#38048=CARTESIAN_POINT('',(-58.5243134690019,-61.2080320947608,-227.49999999998));
#38049=CARTESIAN_POINT('',(-59.753731519493,-43.6265348647336,-235.499999999981));
#38050=CARTESIAN_POINT('Origin',(1.11022302462516E-12,-11.1689999999863,
-227.499999999986));
#38051=CARTESIAN_POINT('',(-32.4575348647341,-70.9227315194864,-227.499999999979));
#38052=CARTESIAN_POINT('',(-50.0390320947626,-69.6933134689986,-227.499999999979));
#38053=CARTESIAN_POINT('',(-33.2449834181943,-70.4882302505881,-227.499999999979));
#38054=CARTESIAN_POINT('Origin',(1.11022302462516E-12,-11.1689999999863,
-227.499999999986));
#38055=CARTESIAN_POINT('',(-49.6843933496171,-69.3386747238527,-227.499999999979));
#38056=CARTESIAN_POINT('',(-33.2449834181943,-70.4882302505881,-227.499999999979));
#38057=CARTESIAN_POINT('',(-58.1696747238564,-60.8533933496149,-227.49999999998));
#38058=CARTESIAN_POINT('Origin',(1.11022302462516E-12,-11.1689999999863,
-227.499999999986));
#38059=CARTESIAN_POINT('',(-59.3192302505947,-44.4139834181924,-227.499999999982));
#38060=CARTESIAN_POINT('',(-59.3192302505947,-44.4139834181924,-227.499999999982));
#38061=CARTESIAN_POINT('Origin',(1.11022302462516E-12,-11.1689999999863,
-227.499999999986));
#38062=CARTESIAN_POINT('Origin',(-50.0390320947626,-69.6933134689995,-235.499999999979));
#38063=CARTESIAN_POINT('',(-32.4575348647341,-70.922731519487,-232.499999999979));
#38064=CARTESIAN_POINT('',(-32.4575348647342,-70.922731519487,-232.499999999979));
#38065=CARTESIAN_POINT('',(-32.4575348647341,-70.9227315194873,-235.499999999979));
#38066=CARTESIAN_POINT('Origin',(-41.9116882454246,-76.0623577133294,-232.499999999978));
#38067=CARTESIAN_POINT('Origin',(1.11022302462516E-12,-11.1689999999869,
-232.499999999986));
#38068=CARTESIAN_POINT('Origin',(-60.650590686874,-36.8087337296458,-207.383019502761));
#38069=CARTESIAN_POINT('Origin',(-6.02295990859147E-12,70.5000000000294,
-92.2599999999947));
#38070=CARTESIAN_POINT('',(4.88675134594208,70.5000000000261,-126.259999999995));
#38071=CARTESIAN_POINT('',(7.7735026918902,70.5000000000257,-131.259999999995));
#38072=CARTESIAN_POINT('',(4.88675134594205,70.5000000000261,-126.259999999995));
#38073=CARTESIAN_POINT('',(4.8867513459421,70.500000000025,-136.259999999995));
#38074=CARTESIAN_POINT('',(7.77350269189023,70.5000000000257,-131.259999999995));
#38075=CARTESIAN_POINT('',(-0.886751345954173,70.5000000000245,-136.259999999995));
#38076=CARTESIAN_POINT('',(4.88675134594208,70.500000000025,-136.259999999995));
#38077=CARTESIAN_POINT('',(-3.77350269190227,70.5000000000247,-131.259999999995));
#38078=CARTESIAN_POINT('',(-0.886751345954173,70.5000000000245,-136.259999999995));
#38079=CARTESIAN_POINT('',(-0.886751345954145,70.5000000000256,-126.259999999995));
#38080=CARTESIAN_POINT('',(-3.77350269190227,70.5000000000247,-131.259999999995));
#38081=CARTESIAN_POINT('',(-0.886751345954145,70.5000000000256,-126.259999999995));
#38082=CARTESIAN_POINT('Origin',(33.2449834182068,-70.48823025058,-207.499999999936));
#38083=CARTESIAN_POINT('',(49.6843933496294,-69.3386747238393,-186.499999999978));
#38084=CARTESIAN_POINT('',(33.2449834182068,-70.48823025058,-207.499999999936));
#38085=CARTESIAN_POINT('Origin',(1.11022302462516E-12,-11.1689999999816,
-186.499999999986));
#38086=CARTESIAN_POINT('',(58.1696747238672,-60.8533933496024,-207.499999999937));
#38087=CARTESIAN_POINT('Origin',(59.3192302506027,-44.4139834181798,-207.499999999939));
#38088=CARTESIAN_POINT('',(59.3192302506028,-44.4139834181829,-235.499999999981));
#38089=CARTESIAN_POINT('Origin',(1.11022302462516E-12,-11.1689999999872,
-235.499999999986));
#38090=CARTESIAN_POINT('',(59.3192302505969,22.075983418222,-207.499999999946));
#38091=CARTESIAN_POINT('Origin',(59.3192302505969,22.075983418222,-207.499999999946));
#38092=CARTESIAN_POINT('',(58.1696747238586,38.515393349647,-186.499999999991));
#38093=CARTESIAN_POINT('Origin',(1.11022302462516E-12,-11.1689999999816,
-186.499999999986));
#38094=CARTESIAN_POINT('',(49.6843933496193,47.0006747238824,-207.499999999949));
#38095=CARTESIAN_POINT('Origin',(33.2449834181965,48.1502302506178,-207.499999999949));
#38096=CARTESIAN_POINT('Origin',(-33.2449834182046,48.150230250612,-207.499999999949));
#38097=CARTESIAN_POINT('',(-49.6843933496272,47.0006747238761,-186.499999999992));
#38098=CARTESIAN_POINT('Origin',(1.11022302462516E-12,-11.1689999999816,
-186.499999999986));
#38099=CARTESIAN_POINT('',(-58.169674723865,38.5153933496345,-207.499999999948));
#38100=CARTESIAN_POINT('Origin',(-59.3192302506005,22.0759834182117,-207.499999999946));
#38101=CARTESIAN_POINT('',(-59.3192302506006,22.0759834182084,-235.499999999989));
#38102=CARTESIAN_POINT('Origin',(1.11022302462516E-12,-11.1689999999872,
-235.499999999986));
#38103=CARTESIAN_POINT('',(-59.3192302505947,-44.41398341819,-207.499999999939));
#38104=CARTESIAN_POINT('Origin',(-59.3192302505947,-44.4139834181901,-207.499999999939));
#38105=CARTESIAN_POINT('',(-58.1696747238564,-60.8533933496102,-186.499999999979));
#38106=CARTESIAN_POINT('Origin',(1.11022302462516E-12,-11.1689999999816,
-186.499999999986));
#38107=CARTESIAN_POINT('',(-49.6843933496171,-69.3386747238504,-207.499999999936));
#38108=CARTESIAN_POINT('Origin',(-33.2449834181943,-70.4882302505858,-207.499999999936));
#38109=CARTESIAN_POINT('',(-33.2449834181943,-70.488230250589,-235.499999999979));
#38110=CARTESIAN_POINT('Origin',(1.11022302462516E-12,-11.1689999999872,
-235.499999999986));
#38111=CARTESIAN_POINT('Origin',(37.489999999994,70.500000000036,-63.2599999999947));
#38112=CARTESIAN_POINT('',(35.999999999994,70.5000000000358,-63.2599999999947));
#38113=CARTESIAN_POINT('',(17.9999999999939,70.5000000000342,-63.2599999999947));
#38114=CARTESIAN_POINT('',(37.489999999994,70.500000000036,-63.2599999999947));
#38115=CARTESIAN_POINT('',(37.489999999994,70.500000000036,-63.2599999999947));
#38116=CARTESIAN_POINT('',(37.489999999994,70.500000000036,-63.2599999999947));
#38117=CARTESIAN_POINT('',(37.489999999994,70.5000000000336,-84.2599999999947));
#38118=CARTESIAN_POINT('',(37.489999999994,70.500000000036,-63.2599999999948));
#38119=CARTESIAN_POINT('',(35.999999999994,70.5000000000335,-84.2599999999948));
#38120=CARTESIAN_POINT('',(37.489999999994,70.5000000000336,-84.2599999999948));
#38121=CARTESIAN_POINT('',(17.9999999999939,70.5000000000319,-84.2599999999948));
#38122=CARTESIAN_POINT('',(37.489999999994,70.5000000000336,-84.2599999999948));
#38123=CARTESIAN_POINT('',(16.489999999994,70.5000000000317,-84.2599999999948));
#38124=CARTESIAN_POINT('',(37.489999999994,70.5000000000336,-84.2599999999947));
#38125=CARTESIAN_POINT('',(16.489999999994,70.5000000000342,-63.2599999999947));
#38126=CARTESIAN_POINT('',(16.489999999994,70.5000000000342,-63.2599999999948));
#38127=CARTESIAN_POINT('',(37.489999999994,70.500000000036,-63.2599999999947));
#38128=CARTESIAN_POINT('Origin',(37.4899999999976,29.8015151901986,-84.2599999999901));
#38129=CARTESIAN_POINT('Origin',(35.999999999995,58.5000000000335,-84.2599999999934));
#38130=CARTESIAN_POINT('Origin',(17.999999999995,58.5000000000319,-84.2599999999934));
#38131=CARTESIAN_POINT('Origin',(16.4999999999975,29.801515190195,-100.25999999999));
#38132=CARTESIAN_POINT('',(35.999999999994,70.5000000000317,-100.259999999995));
#38133=CARTESIAN_POINT('Origin',(35.999999999995,58.5000000000317,-100.259999999993));
#38134=CARTESIAN_POINT('',(17.9999999999939,70.5000000000301,-100.259999999995));
#38135=CARTESIAN_POINT('',(37.4999999999939,70.5000000000318,-100.259999999995));
#38136=CARTESIAN_POINT('Origin',(17.999999999995,58.5000000000301,-100.259999999993));
#38137=CARTESIAN_POINT('Origin',(37.4999999999939,70.5000000000318,-100.259999999995));
#38138=CARTESIAN_POINT('',(37.4999999999939,70.5000000000295,-121.259999999995));
#38139=CARTESIAN_POINT('',(37.4999999999939,70.5000000000319,-100.259999999995));
#38140=CARTESIAN_POINT('',(37.4999999999939,70.5000000000319,-100.259999999995));
#38141=CARTESIAN_POINT('',(35.999999999994,70.5000000000294,-121.259999999995));
#38142=CARTESIAN_POINT('',(16.4999999999939,70.5000000000277,-121.259999999995));
#38143=CARTESIAN_POINT('',(17.9999999999939,70.5000000000278,-121.259999999995));
#38144=CARTESIAN_POINT('',(16.4999999999939,70.5000000000277,-121.259999999995));
#38145=CARTESIAN_POINT('',(16.4999999999939,70.5000000000276,-121.259999999995));
#38146=CARTESIAN_POINT('',(37.4999999999939,70.5000000000295,-121.259999999995));
#38147=CARTESIAN_POINT('',(16.4999999999939,70.50000000003,-100.259999999995));
#38148=CARTESIAN_POINT('',(16.4999999999939,70.50000000003,-100.259999999995));
#38149=CARTESIAN_POINT('',(16.4999999999939,70.50000000003,-100.259999999995));
#38150=CARTESIAN_POINT('',(16.4999999999939,70.50000000003,-100.259999999995));
#38151=CARTESIAN_POINT('Origin',(-6.02295990859147E-12,70.5000000000294,
-92.2599999999947));
#38152=CARTESIAN_POINT('',(4.8867513459421,70.5000000000348,-48.2599999999947));
#38153=CARTESIAN_POINT('',(7.77350269189023,70.5000000000344,-53.2599999999947));
#38154=CARTESIAN_POINT('',(4.88675134594208,70.5000000000348,-48.2599999999946));
#38155=CARTESIAN_POINT('',(4.88675134594208,70.5000000000336,-58.2599999999947));
#38156=CARTESIAN_POINT('',(7.77350269189026,70.5000000000344,-53.2599999999946));
#38157=CARTESIAN_POINT('',(-0.886751345954145,70.5000000000331,-58.2599999999947));
#38158=CARTESIAN_POINT('',(4.88675134594208,70.5000000000336,-58.2599999999947));
#38159=CARTESIAN_POINT('',(-3.7735026919023,70.5000000000334,-53.2599999999947));
#38160=CARTESIAN_POINT('',(-0.886751345954173,70.5000000000331,-58.2599999999946));
#38161=CARTESIAN_POINT('',(-0.886751345954173,70.5000000000343,-48.2599999999947));
#38162=CARTESIAN_POINT('',(-3.77350269190227,70.5000000000334,-53.2599999999946));
#38163=CARTESIAN_POINT('',(-0.886751345954145,70.5000000000343,-48.2599999999946));
#38164=CARTESIAN_POINT('Origin',(-4.96824803519758E-12,58.5000000000244,
-137.259999999993));
#38165=CARTESIAN_POINT('Ctrl Pts',(4.499999999994,69.6242977306701,-121.577541634476));
#38166=CARTESIAN_POINT('Ctrl Pts',(3.69670943613483,69.9492447632731,-121.370132902743));
#38167=CARTESIAN_POINT('Ctrl Pts',(2.8492207351751,70.1886150627173,-121.259999999995));
#38168=CARTESIAN_POINT('Ctrl Pts',(1.3641526653201,70.439637382277,-121.259999999995));
#38169=CARTESIAN_POINT('Ctrl Pts',(0.706314881107781,70.496946126364,-121.32175471629));
#38170=CARTESIAN_POINT('Ctrl Pts',(-0.598427958263334,70.5028113810441,
-121.580614035387));
#38171=CARTESIAN_POINT('Ctrl Pts',(-1.24533966867664,70.4515055296131,-121.777681955094));
#38172=CARTESIAN_POINT('Ctrl Pts',(-2.83779978405687,70.2014113531424,-122.444371841402));
#38173=CARTESIAN_POINT('Ctrl Pts',(-3.73964423272937,69.9318767829018,-123.010297347601));
#38174=CARTESIAN_POINT('Ctrl Pts',(-4.50000000000616,69.6242977306689,-123.660657923209));
#38175=CARTESIAN_POINT('Origin',(-3.7735026919036,85.7752523165442,-131.259999999996));
#38176=CARTESIAN_POINT('',(-3.77350269190194,66.5000000000247,-131.259999999994));
#38177=CARTESIAN_POINT('',(-3.7735026919036,85.7752523165442,-131.259999999996));
#38178=CARTESIAN_POINT('',(-0.886751345953785,66.5000000000256,-126.259999999994));
#38179=CARTESIAN_POINT('',(-3.77350269190197,66.5000000000247,-131.259999999994));
#38180=CARTESIAN_POINT('',(-0.886751345955478,85.775252316545,-126.259999999996));
#38181=CARTESIAN_POINT('Origin',(-0.886751345955478,85.775252316545,-126.259999999996));
#38182=CARTESIAN_POINT('',(4.88675134594241,66.5000000000261,-126.259999999994));
#38183=CARTESIAN_POINT('',(18.1658075373038,66.5000000000273,-126.259999999994));
#38184=CARTESIAN_POINT('',(4.88675134594074,85.7752523165455,-126.259999999996));
#38185=CARTESIAN_POINT('Origin',(4.88675134594074,85.7752523165455,-126.259999999996));
#38186=CARTESIAN_POINT('',(7.77350269189056,66.5000000000257,-131.259999999994));
#38187=CARTESIAN_POINT('',(4.88675134594244,66.5000000000261,-126.259999999994));
#38188=CARTESIAN_POINT('',(7.7735026918889,85.7752523165452,-131.259999999996));
#38189=CARTESIAN_POINT('Origin',(7.77350269188887,85.7752523165452,-131.259999999996));
#38190=CARTESIAN_POINT('',(4.88675134594244,66.5000000000249,-136.259999999994));
#38191=CARTESIAN_POINT('',(7.77350269189056,66.5000000000257,-131.259999999994));
#38192=CARTESIAN_POINT('',(4.88675134594074,85.7752523165443,-136.259999999996));
#38193=CARTESIAN_POINT('Origin',(4.88675134594074,85.7752523165443,-136.259999999996));
#38194=CARTESIAN_POINT('',(-0.886751345953812,66.5000000000244,-136.259999999994));
#38195=CARTESIAN_POINT('',(18.1658075373038,66.5000000000261,-136.259999999994));
#38196=CARTESIAN_POINT('',(-0.886751345955478,85.7752523165438,-136.259999999996));
#38197=CARTESIAN_POINT('Origin',(-0.886751345955478,85.7752523165438,-136.259999999996));
#38198=CARTESIAN_POINT('',(-0.886751345953812,66.5000000000244,-136.259999999994));
#38199=CARTESIAN_POINT('Origin',(1.99999999999398,70.5000000000252,-131.259999999995));
#38200=CARTESIAN_POINT('',(10.6602540378387,66.5000000000266,-126.259999999994));
#38201=CARTESIAN_POINT('',(10.6602540378383,70.5000000000266,-126.259999999995));
#38202=CARTESIAN_POINT('',(-6.66025403785003,66.5000000000251,-126.259999999994));
#38203=CARTESIAN_POINT('Origin',(1.99999999999431,66.5000000000253,-131.259999999994));
#38204=CARTESIAN_POINT('',(-6.66025403785042,70.5000000000251,-126.259999999995));
#38205=CARTESIAN_POINT('Origin',(16.4999999999975,29.8015151901927,-121.25999999999));
#38206=CARTESIAN_POINT('Origin',(35.999999999995,58.5000000000293,-121.259999999993));
#38207=CARTESIAN_POINT('Origin',(17.999999999995,58.5000000000277,-121.259999999993));
#38208=CARTESIAN_POINT('Origin',(1.11022302462516E-13,3.99005915113771E-11,
1.34059430223488E-11));
#38209=CARTESIAN_POINT('Origin',(1.11022302462516E-12,-11.1689999999816,
-186.499999999986));
#38210=CARTESIAN_POINT('Origin',(1.11022302462516E-12,-11.1689999999816,
-186.499999999986));
#38211=CARTESIAN_POINT('Origin',(1.11022302462516E-12,-11.1689999999816,
-186.499999999986));
#38212=CARTESIAN_POINT('Origin',(1.11022302462516E-12,-11.1689999999816,
-186.499999999986));
#38213=CARTESIAN_POINT('Origin',(-54.7313488832587,-33.7472662704153,-202.036058359604));
#38214=CARTESIAN_POINT('',(-60.4268711256452,-32.5555280806013,-200.48984153347));
#38215=CARTESIAN_POINT('',(-55.9721573516798,-38.3905798567208,-205.662355821745));
#38216=CARTESIAN_POINT('Origin',(-58.1950257608648,-35.2740441835029,-203.296733644063));
#38217=CARTESIAN_POINT('Origin',(-58.2040000000278,-35.2780000000023,-203.299999999994));
#38218=CARTESIAN_POINT('Origin',(-56.2373841760092,-35.2780000001109,-208.70323256955));
#38219=CARTESIAN_POINT('',(-61.668735249239,-30.9288598303501,-199.047872363434));
#38220=CARTESIAN_POINT('',(-55.9721573516797,-38.390579856721,-205.662355821745));
#38221=CARTESIAN_POINT('Origin',(-88.6,2.20815119661433E-11,-87.4999999999866));
#38222=CARTESIAN_POINT('',(-88.6,-1.44337567297821,-89.9999999999864));
#38223=CARTESIAN_POINT('',(-88.6,-2.88675134587792,-87.4999999999863));
#38224=CARTESIAN_POINT('',(-88.6,-2.16506350942806,-88.7499999999863));
#38225=CARTESIAN_POINT('',(-88.6,-1.44337567297763,-84.9999999999864));
#38226=CARTESIAN_POINT('',(-88.6,-2.16506350942778,-86.2499999999863));
#38227=CARTESIAN_POINT('',(-88.6,1.44337567302237,-84.9999999999868));
#38228=CARTESIAN_POINT('',(-88.6,2.23590677222995E-11,-84.9999999999866));
#38229=CARTESIAN_POINT('',(-88.6,2.88675134592208,-87.4999999999869));
#38230=CARTESIAN_POINT('',(-88.6,2.16506350947222,-86.2499999999868));
#38231=CARTESIAN_POINT('',(-88.6,1.44337567302179,-89.9999999999867));
#38232=CARTESIAN_POINT('',(-88.6,2.16506350947194,-88.7499999999868));
#38233=CARTESIAN_POINT('',(-88.6,-0.721687836478203,-89.9999999999865));
#38234=CARTESIAN_POINT('Origin',(-6.02295990859147E-12,70.5000000000294,
-92.2599999999947));
#38235=CARTESIAN_POINT('',(-66.1132486540579,70.5000000000198,-126.259999999995));
#38236=CARTESIAN_POINT('',(-63.2264973081098,70.5000000000196,-131.259999999995));
#38237=CARTESIAN_POINT('',(-66.113248654058,70.5000000000198,-126.259999999995));
#38238=CARTESIAN_POINT('',(-66.1132486540579,70.5000000000187,-136.259999999995));
#38239=CARTESIAN_POINT('',(-63.2264973081098,70.5000000000196,-131.259999999995));
#38240=CARTESIAN_POINT('',(-71.8867513459542,70.5000000000182,-136.259999999995));
#38241=CARTESIAN_POINT('',(-66.1132486540579,70.5000000000187,-136.259999999995));
#38242=CARTESIAN_POINT('',(-74.7735026919022,70.5000000000185,-131.259999999995));
#38243=CARTESIAN_POINT('',(-71.8867513459543,70.5000000000182,-136.259999999995));
#38244=CARTESIAN_POINT('',(-71.8867513459541,70.5000000000193,-126.259999999995));
#38245=CARTESIAN_POINT('',(-74.7735026919022,70.5000000000185,-131.259999999995));
#38246=CARTESIAN_POINT('',(-71.8867513459541,70.5000000000194,-126.259999999995));
#38247=CARTESIAN_POINT('Origin',(-6.02295990859147E-12,70.5000000000294,
-92.2599999999947));
#38248=CARTESIAN_POINT('',(-66.1132486540579,70.5000000000286,-48.2599999999947));
#38249=CARTESIAN_POINT('',(-63.2264973081098,70.5000000000283,-53.2599999999947));
#38250=CARTESIAN_POINT('',(-66.113248654058,70.5000000000286,-48.2599999999946));
#38251=CARTESIAN_POINT('',(-66.1132486540579,70.5000000000274,-58.2599999999947));
#38252=CARTESIAN_POINT('',(-63.2264973081098,70.5000000000283,-53.2599999999946));
#38253=CARTESIAN_POINT('',(-71.8867513459541,70.5000000000269,-58.2599999999947));
#38254=CARTESIAN_POINT('',(-66.1132486540579,70.5000000000274,-58.2599999999947));
#38255=CARTESIAN_POINT('',(-74.7735026919022,70.5000000000272,-53.2599999999947));
#38256=CARTESIAN_POINT('',(-71.8867513459542,70.5000000000269,-58.2599999999946));
#38257=CARTESIAN_POINT('',(-71.8867513459541,70.5000000000281,-48.2599999999947));
#38258=CARTESIAN_POINT('',(-74.7735026919022,70.5000000000272,-53.2599999999946));
#38259=CARTESIAN_POINT('',(-71.8867513459541,70.5000000000281,-48.2599999999946));
#38260=CARTESIAN_POINT('Origin',(16.4999999999975,29.8015151901927,-121.25999999999));
#38261=CARTESIAN_POINT('',(37.4999999999939,70.4058808998202,-121.259999999995));
#38262=CARTESIAN_POINT('Origin',(35.999999999995,58.5000000000293,-121.259999999993));
#38263=CARTESIAN_POINT('',(37.4999999999975,29.8015151901944,-121.25999999999));
#38264=CARTESIAN_POINT('Origin',(37.4999999999975,29.8015151901968,-100.25999999999));
#38265=CARTESIAN_POINT('',(37.4999999999939,70.4058808998225,-100.259999999995));
#38266=CARTESIAN_POINT('',(37.4999999999975,29.8015151901968,-100.25999999999));
#38267=CARTESIAN_POINT('',(37.4999999999939,70.4058808998183,-137.259999999995));
#38268=CARTESIAN_POINT('Origin',(16.4999999999975,29.801515190195,-100.25999999999));
#38269=CARTESIAN_POINT('Origin',(35.999999999995,58.5000000000317,-100.259999999993));
#38270=CARTESIAN_POINT('Origin',(37.4899999999976,29.8015151901986,-84.2599999999901));
#38271=CARTESIAN_POINT('',(37.489999999994,70.407136515586,-84.2599999999947));
#38272=CARTESIAN_POINT('Origin',(35.999999999995,58.5000000000335,-84.2599999999934));
#38273=CARTESIAN_POINT('',(37.4899999999976,29.8015151901986,-84.25999999999));
#38274=CARTESIAN_POINT('Origin',(37.4899999999976,29.801515190201,-63.2599999999901));
#38275=CARTESIAN_POINT('',(37.489999999994,70.4071365155883,-63.2599999999947));
#38276=CARTESIAN_POINT('',(37.4899999999976,29.801515190201,-63.2599999999901));
#38277=CARTESIAN_POINT('',(37.489999999994,70.40713651558,-137.259999999995));
#38278=CARTESIAN_POINT('Origin',(37.4899999999976,29.801515190201,-63.2599999999901));
#38279=CARTESIAN_POINT('Origin',(35.999999999995,58.5000000000358,-63.2599999999934));
#38280=CARTESIAN_POINT('Origin',(37.4899999999976,29.801515190201,-63.2599999999901));
#38281=CARTESIAN_POINT('Origin',(35.999999999995,58.5000000000358,-63.2599999999934));
#38282=CARTESIAN_POINT('Origin',(17.999999999995,58.5000000000342,-63.2599999999934));
#38283=CARTESIAN_POINT('Origin',(37.4899999999976,29.801515190201,-63.2599999999901));
#38284=CARTESIAN_POINT('',(16.489999999994,70.4046167515302,-63.2599999999947));
#38285=CARTESIAN_POINT('Origin',(17.999999999995,58.5000000000342,-63.2599999999934));
#38286=CARTESIAN_POINT('',(16.4899999999976,29.8015151901991,-63.25999999999));
#38287=CARTESIAN_POINT('Origin',(16.4899999999976,29.8015151901991,-63.2599999999901));
#38288=CARTESIAN_POINT('',(16.489999999994,70.4046167515278,-84.2599999999947));
#38289=CARTESIAN_POINT('',(16.4899999999976,29.8015151901967,-84.2599999999901));
#38290=CARTESIAN_POINT('',(16.489999999994,70.4046167515219,-137.259999999995));
#38291=CARTESIAN_POINT('Origin',(37.4899999999976,29.8015151901986,-84.2599999999901));
#38292=CARTESIAN_POINT('Origin',(17.999999999995,58.5000000000319,-84.2599999999934));
#38293=CARTESIAN_POINT('Origin',(16.4999999999975,29.801515190195,-100.25999999999));
#38294=CARTESIAN_POINT('',(16.499999999994,70.4058808998207,-100.259999999995));
#38295=CARTESIAN_POINT('Origin',(17.999999999995,58.5000000000301,-100.259999999993));
#38296=CARTESIAN_POINT('',(16.4999999999975,29.801515190195,-100.25999999999));
#38297=CARTESIAN_POINT('Origin',(16.4999999999975,29.801515190195,-100.25999999999));
#38298=CARTESIAN_POINT('',(16.499999999994,70.4058808998183,-121.259999999995));
#38299=CARTESIAN_POINT('',(16.4999999999975,29.8015151901927,-121.25999999999));
#38300=CARTESIAN_POINT('',(16.499999999994,70.4058808998165,-137.259999999995));
#38301=CARTESIAN_POINT('Origin',(16.4999999999975,29.8015151901927,-121.25999999999));
#38302=CARTESIAN_POINT('Origin',(17.999999999995,58.5000000000277,-121.259999999993));
#38303=CARTESIAN_POINT('Origin',(-3.7735026919036,85.7752523165529,-53.2599999999964));
#38304=CARTESIAN_POINT('',(-3.77350269190194,66.5000000000334,-53.2599999999943));
#38305=CARTESIAN_POINT('',(-3.77350269190358,85.7752523165529,-53.2599999999965));
#38306=CARTESIAN_POINT('',(-0.886751345953812,66.5000000000343,-48.2599999999942));
#38307=CARTESIAN_POINT('',(-0.886751345953812,66.5000000000343,-48.2599999999943));
#38308=CARTESIAN_POINT('',(-0.886751345955478,85.7752523165537,-48.2599999999964));
#38309=CARTESIAN_POINT('Origin',(-0.886751345955478,85.7752523165526,-58.2599999999964));
#38310=CARTESIAN_POINT('',(-0.886751345953812,66.5000000000331,-58.2599999999942));
#38311=CARTESIAN_POINT('',(-0.886751345955478,85.7752523165526,-58.2599999999964));
#38312=CARTESIAN_POINT('',(-3.77350269190194,66.5000000000334,-53.2599999999943));
#38313=CARTESIAN_POINT('Origin',(4.88675134594074,85.7752523165531,-58.2599999999964));
#38314=CARTESIAN_POINT('',(4.88675134594244,66.5000000000336,-58.2599999999942));
#38315=CARTESIAN_POINT('',(4.88675134594072,85.7752523165531,-58.2599999999965));
#38316=CARTESIAN_POINT('',(1.99999999999431,66.5000000000334,-58.2599999999943));
#38317=CARTESIAN_POINT('Origin',(7.7735026918889,85.7752523165539,-53.2599999999964));
#38318=CARTESIAN_POINT('',(7.77350269189056,66.5000000000344,-53.2599999999942));
#38319=CARTESIAN_POINT('',(7.77350269188895,85.7752523165538,-53.2599999999965));
#38320=CARTESIAN_POINT('',(4.88675134594244,66.5000000000337,-58.2599999999943));
#38321=CARTESIAN_POINT('Origin',(4.88675134594077,85.7752523165542,-48.2599999999964));
#38322=CARTESIAN_POINT('',(4.88675134594246,66.5000000000348,-48.2599999999942));
#38323=CARTESIAN_POINT('',(4.88675134594077,85.7752523165542,-48.2599999999964));
#38324=CARTESIAN_POINT('',(7.77350269189056,66.5000000000344,-53.2599999999943));
#38325=CARTESIAN_POINT('Origin',(-0.886751345955478,85.7752523165537,-48.2599999999964));
#38326=CARTESIAN_POINT('',(1.99999999999431,66.5000000000345,-48.2599999999943));
#38327=CARTESIAN_POINT('Origin',(-6.66025403785042,70.5000000000251,-126.259999999995));
#38328=CARTESIAN_POINT('',(-12.4337567297464,67.8166247903788,-136.259999999994));
#38329=CARTESIAN_POINT('Origin',(-9.54700538352068,64.4999999997427,-131.259999999512));
#38330=CARTESIAN_POINT('',(-12.4337567297463,66.5000000000234,-136.259999999994));
#38331=CARTESIAN_POINT('',(-6.66025403785006,66.5000000000251,-126.259999999994));
#38332=CARTESIAN_POINT('',(-12.4337567297467,70.5000000000234,-136.259999999995));
#38333=CARTESIAN_POINT('Origin',(-14.1658075373155,70.5000000000234,-135.259999999995));
#38334=CARTESIAN_POINT('',(-13.0456138058833,66.5000000000233,-136.916854249487));
#38335=CARTESIAN_POINT('Origin',(-14.1658075373152,66.5000000000234,-135.259999999994));
#38336=CARTESIAN_POINT('Ctrl Pts',(-12.4337567297465,67.8166247903788,-136.259999999994));
#38337=CARTESIAN_POINT('Ctrl Pts',(-12.527412483404,67.5720741794269,-136.42221652375));
#38338=CARTESIAN_POINT('Ctrl Pts',(-12.6384034068036,67.3227889604539,-136.561022994229));
#38339=CARTESIAN_POINT('Ctrl Pts',(-12.8407204020393,66.8991702874016,-136.763339989465));
#38340=CARTESIAN_POINT('Ctrl Pts',(-12.9396941466076,66.7025491386428,-136.845242314766));
#38341=CARTESIAN_POINT('Ctrl Pts',(-13.0456138058835,66.5000000000234,-136.916854249487));
#38342=CARTESIAN_POINT('Origin',(18.1658075373038,66.5000000000262,-135.259999999994));
#38343=CARTESIAN_POINT('',(16.4337567297349,66.5000000000259,-136.259999999994));
#38344=CARTESIAN_POINT('',(16.4337567297349,66.5000000000259,-136.259999999994));
#38345=CARTESIAN_POINT('',(17.0456138058719,66.500000000026,-136.916854249486));
#38346=CARTESIAN_POINT('Origin',(18.1658075373038,66.5000000000262,-135.259999999994));
#38347=CARTESIAN_POINT('',(74.4999999999943,66.500000000031,-136.916854249487));
#38348=CARTESIAN_POINT('Origin',(18.1658075373035,70.5000000000262,-135.259999999995));
#38349=CARTESIAN_POINT('',(16.4337567297348,67.8166247903813,-136.259999999994));
#38350=CARTESIAN_POINT('',(16.4337567297346,70.5000000000259,-136.259999999995));
#38351=CARTESIAN_POINT('Ctrl Pts',(17.0456138058721,66.5000000000261,-136.916854249487));
#38352=CARTESIAN_POINT('Ctrl Pts',(16.9396941465962,66.7025491386454,-136.845242314766));
#38353=CARTESIAN_POINT('Ctrl Pts',(16.8407204020279,66.8991702874042,-136.763339989465));
#38354=CARTESIAN_POINT('Ctrl Pts',(16.6384034067921,67.3227889604565,-136.561022994229));
#38355=CARTESIAN_POINT('Ctrl Pts',(16.5274124833925,67.5720741794294,-136.42221652375));
#38356=CARTESIAN_POINT('Ctrl Pts',(16.4337567297349,67.8166247903813,-136.259999999994));
#38357=CARTESIAN_POINT('Origin',(16.4337567297346,70.5000000000259,-136.259999999995));
#38358=CARTESIAN_POINT('',(14.8295692198259,70.0736065540853,-133.481465727965));
#38359=CARTESIAN_POINT('Origin',(17.9999999908615,58.5000000268696,-138.972812905301));
#38360=CARTESIAN_POINT('Origin',(13.5470053838188,64.5000000000939,-131.260000000049));
#38361=CARTESIAN_POINT('Origin',(-6.02295990859147E-12,70.5000000000294,
-92.2599999999947));
#38362=CARTESIAN_POINT('',(71.8867513459421,70.5000000000319,-126.259999999995));
#38363=CARTESIAN_POINT('',(74.7735026918903,70.5000000000316,-131.259999999995));
#38364=CARTESIAN_POINT('',(71.8867513459421,70.5000000000319,-126.259999999995));
#38365=CARTESIAN_POINT('',(71.8867513459421,70.5000000000308,-136.259999999995));
#38366=CARTESIAN_POINT('',(74.7735026918903,70.5000000000316,-131.259999999995));
#38367=CARTESIAN_POINT('',(66.1132486540459,70.5000000000303,-136.259999999995));
#38368=CARTESIAN_POINT('',(71.8867513459421,70.5000000000308,-136.259999999995));
#38369=CARTESIAN_POINT('',(63.2264973080978,70.5000000000306,-131.259999999995));
#38370=CARTESIAN_POINT('',(66.1132486540459,70.5000000000303,-136.259999999995));
#38371=CARTESIAN_POINT('',(66.1132486540459,70.5000000000314,-126.259999999995));
#38372=CARTESIAN_POINT('',(63.2264973080978,70.5000000000306,-131.259999999995));
#38373=CARTESIAN_POINT('',(66.1132486540459,70.5000000000314,-126.259999999995));
#38374=CARTESIAN_POINT('Origin',(-6.02295990859147E-12,70.5000000000294,
-92.2599999999947));
#38375=CARTESIAN_POINT('',(71.8867513459421,70.5000000000406,-48.2599999999947));
#38376=CARTESIAN_POINT('',(74.7735026918903,70.5000000000403,-53.2599999999947));
#38377=CARTESIAN_POINT('',(71.8867513459421,70.5000000000406,-48.2599999999946));
#38378=CARTESIAN_POINT('',(71.8867513459421,70.5000000000394,-58.2599999999947));
#38379=CARTESIAN_POINT('',(74.7735026918903,70.5000000000403,-53.2599999999946));
#38380=CARTESIAN_POINT('',(66.1132486540459,70.5000000000389,-58.2599999999947));
#38381=CARTESIAN_POINT('',(71.8867513459421,70.5000000000394,-58.2599999999947));
#38382=CARTESIAN_POINT('',(63.2264973080978,70.5000000000393,-53.2599999999947));
#38383=CARTESIAN_POINT('',(66.1132486540459,70.5000000000389,-58.2599999999946));
#38384=CARTESIAN_POINT('',(66.1132486540459,70.5000000000401,-48.2599999999947));
#38385=CARTESIAN_POINT('',(63.2264973080978,70.5000000000393,-53.2599999999946));
#38386=CARTESIAN_POINT('',(66.1132486540459,70.5000000000401,-48.2599999999946));
#38387=CARTESIAN_POINT('Origin',(88.6000000000047,-51.9999999999593,-60.4999999999806));
#38388=CARTESIAN_POINT('',(88.6000000000048,-53.4433756729591,-57.9999999999804));
#38389=CARTESIAN_POINT('',(88.6000000000049,-54.8867513458593,-60.4999999999803));
#38390=CARTESIAN_POINT('',(88.6000000000049,-54.1650635094092,-59.2499999999804));
#38391=CARTESIAN_POINT('',(88.6000000000048,-53.4433756729596,-62.9999999999804));
#38392=CARTESIAN_POINT('',(88.6000000000049,-54.1650635094095,-61.7499999999804));
#38393=CARTESIAN_POINT('',(88.6000000000045,-50.5566243269596,-62.9999999999808));
#38394=CARTESIAN_POINT('',(88.6000000000047,-52.7216878364596,-62.9999999999805));
#38395=CARTESIAN_POINT('',(88.6000000000044,-49.1132486540593,-60.4999999999809));
#38396=CARTESIAN_POINT('',(88.6000000000045,-49.8349364905095,-61.7499999999809));
#38397=CARTESIAN_POINT('',(88.6000000000045,-50.5566243269591,-57.9999999999808));
#38398=CARTESIAN_POINT('',(88.6000000000045,-49.8349364905092,-59.2499999999809));
#38399=CARTESIAN_POINT('',(88.6000000000047,-51.999999999959,-57.9999999999806));
#38400=CARTESIAN_POINT('Origin',(-44.5975847992976,-39.383454275573,-196.399999999982));
#38401=CARTESIAN_POINT('',(-57.0363320232113,-44.53575207465,-196.499999999982));
#38402=CARTESIAN_POINT('',(-44.8103167727357,-39.4715707441215,-196.499999999982));
#38403=CARTESIAN_POINT('',(-51.9295288153114,-42.4204449255687,-211.686857166484));
#38404=CARTESIAN_POINT('Origin',(-58.8178305978845,-25.7906133403662,-211.686857166486));
#38405=CARTESIAN_POINT('',(-63.9246338057844,-27.9059204894474,-196.499999999984));
#38406=CARTESIAN_POINT('',(-57.0363320232113,-44.53575207465,-196.499999999982));
#38407=CARTESIAN_POINT('',(-63.9246338057844,-27.9059204894474,-196.499999999984));
#38408=CARTESIAN_POINT('Origin',(-51.4858865818706,-22.7536226903704,-196.399999999984));
#38409=CARTESIAN_POINT('',(-63.9246338057844,-27.9059204894474,-196.499999999984));
#38410=CARTESIAN_POINT('Origin',(-66.0000000000025,29.5000000000287,-47.29999999999));
#38411=CARTESIAN_POINT('',(-68.5000000000023,28.0566243270285,-47.2999999999898));
#38412=CARTESIAN_POINT('',(-66.0000000000022,26.6132486541287,-47.2999999999897));
#38413=CARTESIAN_POINT('',(-67.2500000000023,27.3349364905786,-47.2999999999897));
#38414=CARTESIAN_POINT('',(-63.5000000000023,28.0566243270289,-47.2999999999898));
#38415=CARTESIAN_POINT('',(-64.7500000000023,27.3349364905788,-47.2999999999897));
#38416=CARTESIAN_POINT('',(-63.5000000000026,30.9433756730289,-47.2999999999902));
#38417=CARTESIAN_POINT('',(-63.5000000000025,29.5000000000289,-47.29999999999));
#38418=CARTESIAN_POINT('',(-66.0000000000027,32.3867513459287,-47.2999999999903));
#38419=CARTESIAN_POINT('',(-64.7500000000026,31.6650635094788,-47.2999999999902));
#38420=CARTESIAN_POINT('',(-68.5000000000026,30.9433756730285,-47.2999999999902));
#38421=CARTESIAN_POINT('',(-67.2500000000026,31.6650635094786,-47.2999999999902));
#38422=CARTESIAN_POINT('',(-68.5000000000024,28.7783121635285,-47.2999999999899));
#38423=CARTESIAN_POINT('Origin',(88.2000000000047,-51.9999999999594,-60.4999999999806));
#38424=CARTESIAN_POINT('',(88.2000000000048,-53.4433756729597,-62.9999999999804));
#38425=CARTESIAN_POINT('',(88.2000000000049,-54.8867513458594,-60.4999999999803));
#38426=CARTESIAN_POINT('',(88.2000000000049,-54.1650635094095,-61.7499999999804));
#38427=CARTESIAN_POINT('',(88.2000000000048,-53.4433756729591,-57.9999999999804));
#38428=CARTESIAN_POINT('',(88.2000000000049,-54.1650635094092,-59.2499999999804));
#38429=CARTESIAN_POINT('',(88.2000000000045,-50.5566243269591,-57.9999999999808));
#38430=CARTESIAN_POINT('',(88.2000000000047,-51.9999999999591,-57.9999999999806));
#38431=CARTESIAN_POINT('',(88.2000000000044,-49.1132486540594,-60.4999999999809));
#38432=CARTESIAN_POINT('',(88.2000000000045,-49.8349364905093,-59.2499999999809));
#38433=CARTESIAN_POINT('',(88.2000000000045,-50.5566243269597,-62.9999999999808));
#38434=CARTESIAN_POINT('',(88.2000000000045,-49.8349364905095,-61.7499999999809));
#38435=CARTESIAN_POINT('',(88.2000000000047,-52.7216878364597,-62.9999999999805));
#38436=CARTESIAN_POINT('Origin',(-92.6,-0.721687836478536,-89.9999999999865));
#38437=CARTESIAN_POINT('',(-92.4,-1.44337567297854,-89.9999999999864));
#38438=CARTESIAN_POINT('',(-92.6,-1.44337567297854,-89.9999999999864));
#38439=CARTESIAN_POINT('',(-92.4,1.44337567302146,-89.9999999999867));
#38440=CARTESIAN_POINT('',(-92.6,1.44337567302146,-89.9999999999867));
#38441=CARTESIAN_POINT('',(-92.4,2.14708893025995E-11,-89.9999999999866));
#38442=CARTESIAN_POINT('Origin',(-92.6,2.16506350947161,-88.7499999999868));
#38443=CARTESIAN_POINT('',(-92.4,2.88675134592174,-87.4999999999869));
#38444=CARTESIAN_POINT('',(-92.6,2.88675134592174,-87.4999999999869));
#38445=CARTESIAN_POINT('',(-92.4,1.44337567302146,-89.9999999999867));
#38446=CARTESIAN_POINT('Origin',(-92.6,2.16506350947189,-86.2499999999868));
#38447=CARTESIAN_POINT('',(-92.4,1.44337567302204,-84.9999999999868));
#38448=CARTESIAN_POINT('',(-92.6,1.44337567302204,-84.9999999999868));
#38449=CARTESIAN_POINT('',(-92.4,2.88675134592174,-87.4999999999869));
#38450=CARTESIAN_POINT('Origin',(-92.6,2.2026000814912E-11,-84.9999999999866));
#38451=CARTESIAN_POINT('',(-92.4,-1.44337567297796,-84.9999999999864));
#38452=CARTESIAN_POINT('',(-92.6,-1.44337567297796,-84.9999999999864));
#38453=CARTESIAN_POINT('',(-92.4,2.2026000814912E-11,-84.9999999999866));
#38454=CARTESIAN_POINT('Origin',(-92.6,-2.16506350942812,-86.2499999999863));
#38455=CARTESIAN_POINT('',(-92.4,-2.88675134587825,-87.4999999999863));
#38456=CARTESIAN_POINT('',(-92.6,-2.88675134587825,-87.4999999999863));
#38457=CARTESIAN_POINT('',(-92.4,-1.44337567297796,-84.9999999999864));
#38458=CARTESIAN_POINT('Origin',(-92.6,-2.16506350942839,-88.7499999999863));
#38459=CARTESIAN_POINT('',(-92.4,-2.88675134587825,-87.4999999999863));
#38460=CARTESIAN_POINT('Origin',(-59.000000000006,70.5000000000192,-137.259999999995));
#38461=CARTESIAN_POINT('',(-59.0000000000057,66.50000000002,-131.259999999994));
#38462=CARTESIAN_POINT('',(-59.0000000000061,70.50000000002,-131.259999999995));
#38463=CARTESIAN_POINT('',(-59.0000000000061,70.5000000000199,-131.259999999995));
#38464=CARTESIAN_POINT('',(-59.0000000000057,66.5000000000193,-136.916854249486));
#38465=CARTESIAN_POINT('Origin',(-59.0000000000055,64.5000000000199,-131.259999999994));
#38466=CARTESIAN_POINT('',(-59.0000000000057,66.5000000000199,-131.259999999994));
#38467=CARTESIAN_POINT('Origin',(-69.000000000006,70.5000000000191,-131.259999999995));
#38468=CARTESIAN_POINT('',(-69.000000000006,70.5000000000203,-121.259999999995));
#38469=CARTESIAN_POINT('',(-69.0000000000057,66.5000000000203,-121.259999999994));
#38470=CARTESIAN_POINT('',(-69.000000000006,70.5000000000202,-121.259999999995));
#38471=CARTESIAN_POINT('Origin',(-69.000000000006,70.5000000000191,-131.259999999995));
#38472=CARTESIAN_POINT('Origin',(-69.0000000000057,66.5000000000191,-131.259999999994));
#38473=CARTESIAN_POINT('Origin',(-69.000000000006,70.5000000000202,-121.259999999995));
#38474=CARTESIAN_POINT('',(-77.0000000000057,66.5000000000195,-121.259999999994));
#38475=CARTESIAN_POINT('',(-69.0000000000057,66.5000000000202,-121.259999999994));
#38476=CARTESIAN_POINT('',(-77.0000000000058,68.0000000000195,-121.259999999994));
#38477=CARTESIAN_POINT('',(-77.000000000006,70.5000000000195,-121.259999999995));
#38478=CARTESIAN_POINT('',(-74.500000000006,70.5000000000197,-121.259999999995));
#38479=CARTESIAN_POINT('Origin',(-74.5000000000058,68.0000000000197,-121.259999999994));
#38480=CARTESIAN_POINT('',(74.499999999994,70.5000000000327,-121.259999999995));
#38481=CARTESIAN_POINT('Origin',(-74.7735026919036,85.7752523165379,-131.259999999996));
#38482=CARTESIAN_POINT('',(-74.7735026919019,66.5000000000185,-131.259999999994));
#38483=CARTESIAN_POINT('',(-74.7735026919037,85.775252316538,-131.259999999996));
#38484=CARTESIAN_POINT('',(-71.8867513459538,66.5000000000193,-126.259999999994));
#38485=CARTESIAN_POINT('',(-74.7735026919019,66.5000000000185,-131.259999999994));
#38486=CARTESIAN_POINT('',(-71.8867513459555,85.7752523165388,-126.259999999996));
#38487=CARTESIAN_POINT('Origin',(-71.8867513459555,85.7752523165388,-126.259999999996));
#38488=CARTESIAN_POINT('',(-66.1132486540576,66.5000000000198,-126.259999999994));
#38489=CARTESIAN_POINT('',(-69.0000000000057,66.5000000000197,-126.259999999994));
#38490=CARTESIAN_POINT('',(-66.1132486540593,85.7752523165393,-126.259999999996));
#38491=CARTESIAN_POINT('Origin',(-66.1132486540593,85.7752523165393,-126.259999999996));
#38492=CARTESIAN_POINT('',(-63.2264973081095,66.5000000000196,-131.259999999994));
#38493=CARTESIAN_POINT('',(-66.1132486540576,66.5000000000199,-126.259999999994));
#38494=CARTESIAN_POINT('',(-63.2264973081112,85.775252316539,-131.259999999996));
#38495=CARTESIAN_POINT('Origin',(-63.2264973081112,85.775252316539,-131.259999999996));
#38496=CARTESIAN_POINT('',(-66.1132486540576,66.5000000000187,-136.259999999994));
#38497=CARTESIAN_POINT('',(-63.2264973081095,66.5000000000196,-131.259999999994));
#38498=CARTESIAN_POINT('',(-66.1132486540593,85.7752523165382,-136.259999999996));
#38499=CARTESIAN_POINT('Origin',(-66.1132486540593,85.7752523165382,-136.259999999996));
#38500=CARTESIAN_POINT('',(-71.8867513459539,66.5000000000182,-136.259999999994));
#38501=CARTESIAN_POINT('',(-69.0000000000057,66.5000000000185,-136.259999999994));
#38502=CARTESIAN_POINT('',(-71.8867513459556,85.7752523165377,-136.259999999996));
#38503=CARTESIAN_POINT('Origin',(-71.8867513459556,85.7752523165377,-136.259999999996));
#38504=CARTESIAN_POINT('',(-71.8867513459539,66.5000000000182,-136.259999999994));
#38505=CARTESIAN_POINT('Origin',(-69.000000000006,70.5000000000279,-53.2599999999947));
#38506=CARTESIAN_POINT('',(-59.0000000000061,70.5000000000287,-53.2599999999947));
#38507=CARTESIAN_POINT('',(-59.0000000000057,66.5000000000286,-53.2599999999943));
#38508=CARTESIAN_POINT('',(-59.0000000000061,70.5000000000286,-53.2599999999947));
#38509=CARTESIAN_POINT('',(-69.000000000006,70.5000000000268,-63.2599999999947));
#38510=CARTESIAN_POINT('Origin',(-69.000000000006,70.5000000000278,-53.2599999999947));
#38511=CARTESIAN_POINT('',(-69.0000000000057,66.5000000000267,-63.2599999999943));
#38512=CARTESIAN_POINT('',(-69.000000000006,70.5000000000267,-63.2599999999947));
#38513=CARTESIAN_POINT('Origin',(-69.0000000000057,66.5000000000278,-53.2599999999943));
#38514=CARTESIAN_POINT('Origin',(-69.000000000006,70.5000000000267,-63.2599999999947));
#38515=CARTESIAN_POINT('',(-74.500000000006,70.5000000000262,-63.2599999999947));
#38516=CARTESIAN_POINT('',(74.499999999994,70.5000000000394,-63.2599999999947));
#38517=CARTESIAN_POINT('',(-77.0000000000058,68.000000000026,-63.2599999999944));
#38518=CARTESIAN_POINT('Origin',(-74.5000000000058,68.000000000026,-63.2599999999944));
#38519=CARTESIAN_POINT('',(-77.0000000000057,66.5000000000259,-63.2599999999942));
#38520=CARTESIAN_POINT('',(-77.000000000006,70.500000000026,-63.2599999999947));
#38521=CARTESIAN_POINT('',(-69.0000000000057,66.5000000000267,-63.2599999999942));
#38522=CARTESIAN_POINT('Origin',(-74.7735026919036,85.7752523165467,-53.2599999999964));
#38523=CARTESIAN_POINT('',(-74.7735026919019,66.5000000000272,-53.2599999999943));
#38524=CARTESIAN_POINT('',(-74.7735026919035,85.7752523165467,-53.2599999999965));
#38525=CARTESIAN_POINT('',(-71.8867513459538,66.5000000000281,-48.2599999999942));
#38526=CARTESIAN_POINT('',(-71.8867513459538,66.5000000000281,-48.2599999999943));
#38527=CARTESIAN_POINT('',(-71.8867513459555,85.7752523165475,-48.2599999999964));
#38528=CARTESIAN_POINT('Origin',(-71.8867513459555,85.7752523165464,-58.2599999999964));
#38529=CARTESIAN_POINT('',(-71.8867513459538,66.5000000000269,-58.2599999999942));
#38530=CARTESIAN_POINT('',(-71.8867513459555,85.7752523165464,-58.2599999999964));
#38531=CARTESIAN_POINT('',(-74.7735026919019,66.5000000000272,-53.2599999999943));
#38532=CARTESIAN_POINT('Origin',(-66.1132486540593,85.7752523165469,-58.2599999999964));
#38533=CARTESIAN_POINT('',(-66.1132486540576,66.5000000000274,-58.2599999999942));
#38534=CARTESIAN_POINT('',(-66.1132486540593,85.7752523165469,-58.2599999999964));
#38535=CARTESIAN_POINT('',(-69.0000000000057,66.5000000000272,-58.2599999999943));
#38536=CARTESIAN_POINT('Origin',(-63.2264973081112,85.7752523165478,-53.2599999999964));
#38537=CARTESIAN_POINT('',(-63.2264973081095,66.5000000000283,-53.2599999999942));
#38538=CARTESIAN_POINT('',(-63.2264973081111,85.7752523165477,-53.2599999999965));
#38539=CARTESIAN_POINT('',(-66.1132486540576,66.5000000000274,-58.2599999999943));
#38540=CARTESIAN_POINT('Origin',(-66.1132486540593,85.775252316548,-48.2599999999964));
#38541=CARTESIAN_POINT('',(-66.1132486540576,66.5000000000286,-48.2599999999942));
#38542=CARTESIAN_POINT('',(-66.1132486540593,85.775252316548,-48.2599999999964));
#38543=CARTESIAN_POINT('',(-63.2264973081095,66.5000000000283,-53.2599999999943));
#38544=CARTESIAN_POINT('Origin',(-71.8867513459555,85.7752523165475,-48.2599999999964));
#38545=CARTESIAN_POINT('',(-69.0000000000057,66.5000000000283,-48.2599999999943));
#38546=CARTESIAN_POINT('Origin',(53.999999999995,58.5000000000291,-137.259999999993));
#38547=CARTESIAN_POINT('',(53.999999999994,70.5000000000387,-53.2599999999947));
#38548=CARTESIAN_POINT('',(53.999999999994,70.5000000000298,-131.259999999995));
#38549=CARTESIAN_POINT('',(53.999999999994,70.5000000000291,-137.259999999995));
#38550=CARTESIAN_POINT('Ctrl Pts',(49.4999999999941,69.6242977306726,-134.381149270331));
#38551=CARTESIAN_POINT('Ctrl Pts',(49.8539422620161,69.7674744252977,-134.146082008947));
#38552=CARTESIAN_POINT('Ctrl Pts',(50.2140176820507,69.8933981532635,-133.902800848474));
#38553=CARTESIAN_POINT('Ctrl Pts',(51.7309088331643,70.3448922127441,-132.865641552744));
#38554=CARTESIAN_POINT('Ctrl Pts',(52.913589003477,70.5000000000296,-132.028208582787));
#38555=CARTESIAN_POINT('Ctrl Pts',(53.999999999994,70.5000000000298,-131.259999999995));
#38556=CARTESIAN_POINT('Ctrl Pts',(53.999999999994,70.5000000000385,-53.2599999999947));
#38557=CARTESIAN_POINT('Ctrl Pts',(52.913589003477,70.5000000000385,-52.4917914172019));
#38558=CARTESIAN_POINT('Ctrl Pts',(51.7309088331643,70.3448922127531,-51.6543584472452));
#38559=CARTESIAN_POINT('Ctrl Pts',(50.2140176820507,69.8933981532728,-50.617199151515));
#38560=CARTESIAN_POINT('Ctrl Pts',(49.8539422620161,69.7674744253071,-50.373917991042));
#38561=CARTESIAN_POINT('Ctrl Pts',(49.4999999999941,69.624297730682,-50.1388507296581));
#38562=CARTESIAN_POINT('Origin',(35.999999999995,58.5000000000275,-137.259999999993));
#38563=CARTESIAN_POINT('',(35.999999999994,70.5000000000369,-53.2599999999947));
#38564=CARTESIAN_POINT('Ctrl Pts',(35.999999999994,70.500000000037,-53.2599999999947));
#38565=CARTESIAN_POINT('Ctrl Pts',(34.913589003477,70.5000000000369,-52.4917914172019));
#38566=CARTESIAN_POINT('Ctrl Pts',(33.7309088331644,70.3448922127515,-51.6543584472451));
#38567=CARTESIAN_POINT('Ctrl Pts',(32.2140176820507,69.8933981532712,-50.6171991515149));
#38568=CARTESIAN_POINT('Ctrl Pts',(31.8539422620161,69.7674744253055,-50.3739179910419));
#38569=CARTESIAN_POINT('Ctrl Pts',(31.4999999999941,69.6242977306804,-50.138850729658));
#38570=CARTESIAN_POINT('Ctrl Pts',(40.499999999994,69.6242977306811,-50.138850729658));
#38571=CARTESIAN_POINT('Ctrl Pts',(40.146057737972,69.7674744253062,-50.3739179910419));
#38572=CARTESIAN_POINT('Ctrl Pts',(39.7859823179373,69.8933981532718,-50.6171991515149));
#38573=CARTESIAN_POINT('Ctrl Pts',(38.2690911668236,70.3448922127519,-51.6543584472451));
#38574=CARTESIAN_POINT('Ctrl Pts',(37.0864109965109,70.5000000000371,-52.4917914172019));
#38575=CARTESIAN_POINT('Ctrl Pts',(35.999999999994,70.500000000037,-53.2599999999947));
#38576=CARTESIAN_POINT('',(35.999999999994,70.5000000000282,-131.259999999995));
#38577=CARTESIAN_POINT('Ctrl Pts',(35.999999999994,70.5000000000283,-131.259999999995));
#38578=CARTESIAN_POINT('Ctrl Pts',(37.0864109965109,70.5000000000283,-132.028208582787));
#38579=CARTESIAN_POINT('Ctrl Pts',(38.2690911668235,70.3448922127429,-132.865641552744));
#38580=CARTESIAN_POINT('Ctrl Pts',(39.7859823179373,69.8933981532626,-133.902800848474));
#38581=CARTESIAN_POINT('Ctrl Pts',(40.1460577379719,69.7674744252968,-134.146082008947));
#38582=CARTESIAN_POINT('Ctrl Pts',(40.4999999999939,69.6242977306718,-134.381149270331));
#38583=CARTESIAN_POINT('Ctrl Pts',(31.4999999999942,69.624297730671,-134.381149270331));
#38584=CARTESIAN_POINT('Ctrl Pts',(31.8539422620161,69.7674744252961,-134.146082008947));
#38585=CARTESIAN_POINT('Ctrl Pts',(32.2140176820507,69.8933981532619,-133.902800848474));
#38586=CARTESIAN_POINT('Ctrl Pts',(33.7309088331644,70.3448922127425,-132.865641552744));
#38587=CARTESIAN_POINT('Ctrl Pts',(34.913589003477,70.5000000000281,-132.028208582787));
#38588=CARTESIAN_POINT('Ctrl Pts',(35.999999999994,70.5000000000283,-131.259999999995));
#38589=CARTESIAN_POINT('Origin',(17.999999999995,58.5000000000259,-137.259999999993));
#38590=CARTESIAN_POINT('',(17.9999999999939,70.5000000000266,-131.259999999995));
#38591=CARTESIAN_POINT('Ctrl Pts',(17.999999999994,70.5000000000267,-131.259999999995));
#38592=CARTESIAN_POINT('Ctrl Pts',(19.0864109965109,70.5000000000267,-132.028208582787));
#38593=CARTESIAN_POINT('Ctrl Pts',(20.2690911668235,70.3448922127413,-132.865641552744));
#38594=CARTESIAN_POINT('Ctrl Pts',(21.7859823179372,69.893398153261,-133.902800848474));
#38595=CARTESIAN_POINT('Ctrl Pts',(22.1460577379719,69.7674744252952,-134.146082008947));
#38596=CARTESIAN_POINT('Ctrl Pts',(22.4999999999939,69.6242977306702,-134.381149270331));
#38597=CARTESIAN_POINT('Ctrl Pts',(14.829569219826,70.0736065540853,-133.481465727965));
#38598=CARTESIAN_POINT('Ctrl Pts',(15.9026718230638,70.3675682943341,-132.743922464767));
#38599=CARTESIAN_POINT('Ctrl Pts',(16.9928110658882,70.5000000000265,-131.972190125237));
#38600=CARTESIAN_POINT('Ctrl Pts',(17.999999999994,70.5000000000267,-131.259999999995));
#38601=CARTESIAN_POINT('',(14.8295692198259,70.0736065540945,-51.038534272024));
#38602=CARTESIAN_POINT('Origin',(17.9999999898631,58.5000000290889,-45.547187096471));
#38603=CARTESIAN_POINT('',(17.9999999999939,70.5000000000353,-53.2599999999947));
#38604=CARTESIAN_POINT('Ctrl Pts',(17.999999999994,70.5000000000354,-53.2599999999947));
#38605=CARTESIAN_POINT('Ctrl Pts',(16.9928110658882,70.5000000000354,-52.5478098747524));
#38606=CARTESIAN_POINT('Ctrl Pts',(15.9026718230638,70.3675682943431,-51.7760775352227));
#38607=CARTESIAN_POINT('Ctrl Pts',(14.829569219826,70.0736065540945,-51.0385342720238));
#38608=CARTESIAN_POINT('Ctrl Pts',(22.499999999994,69.6242977306796,-50.138850729658));
#38609=CARTESIAN_POINT('Ctrl Pts',(22.146057737972,69.7674744253046,-50.3739179910419));
#38610=CARTESIAN_POINT('Ctrl Pts',(21.7859823179373,69.8933981532703,-50.6171991515149));
#38611=CARTESIAN_POINT('Ctrl Pts',(20.2690911668235,70.3448922127504,-51.654358447245));
#38612=CARTESIAN_POINT('Ctrl Pts',(19.0864109965109,70.5000000000356,-52.4917914172019));
#38613=CARTESIAN_POINT('Ctrl Pts',(17.999999999994,70.5000000000354,-53.2599999999947));
#38614=CARTESIAN_POINT('Origin',(16.4337567297346,70.5000000000358,-48.2599999999947));
#38615=CARTESIAN_POINT('',(16.4337567297348,67.8166247903912,-48.2599999999944));
#38616=CARTESIAN_POINT('',(16.4337567297349,66.5000000000358,-48.2599999999943));
#38617=CARTESIAN_POINT('',(16.4337567297346,70.5000000000358,-48.2599999999947));
#38618=CARTESIAN_POINT('Origin',(13.5470053837932,64.5000000000491,-53.2599999999832));
#38619=CARTESIAN_POINT('',(16.4337567297349,66.5000000000358,-48.2599999999943));
#38620=CARTESIAN_POINT('Origin',(18.1658075373035,70.5000000000358,-49.2599999999947));
#38621=CARTESIAN_POINT('',(17.0456138058721,66.5000000000359,-47.6031457505019));
#38622=CARTESIAN_POINT('Origin',(18.1658075373038,66.5000000000358,-49.2599999999943));
#38623=CARTESIAN_POINT('Ctrl Pts',(16.4337567297349,67.8166247903912,-48.2599999999944));
#38624=CARTESIAN_POINT('Ctrl Pts',(16.5274124833924,67.5720741794393,-48.0977834762383));
#38625=CARTESIAN_POINT('Ctrl Pts',(16.6384034067921,67.3227889604663,-47.9589770057598));
#38626=CARTESIAN_POINT('Ctrl Pts',(16.8407204020279,66.8991702874141,-47.756660010524));
#38627=CARTESIAN_POINT('Ctrl Pts',(16.9396941465962,66.7025491386553,-47.6747576852225));
#38628=CARTESIAN_POINT('Ctrl Pts',(17.0456138058721,66.500000000036,-47.6031457505018));
#38629=CARTESIAN_POINT('Origin',(1.99999999999431,66.5000000000339,-53.2599999999943));
#38630=CARTESIAN_POINT('',(-13.0456138058834,66.5000000000333,-47.6031457505019));
#38631=CARTESIAN_POINT('',(-12.4337567297463,66.5000000000332,-48.2599999999943));
#38632=CARTESIAN_POINT('Origin',(-14.1658075373152,66.500000000033,-49.2599999999943));
#38633=CARTESIAN_POINT('',(74.4999999999943,66.5000000000409,-47.6031457505019));
#38634=CARTESIAN_POINT('',(-6.66025403785006,66.5000000000326,-58.2599999999943));
#38635=CARTESIAN_POINT('Origin',(-14.1658075373155,70.500000000033,-49.2599999999947));
#38636=CARTESIAN_POINT('',(-12.4337567297464,67.8166247903887,-48.2599999999944));
#38637=CARTESIAN_POINT('',(-12.4337567297466,70.5000000000333,-48.2599999999947));
#38638=CARTESIAN_POINT('Ctrl Pts',(-13.0456138058834,66.5000000000333,-47.6031457505018));
#38639=CARTESIAN_POINT('Ctrl Pts',(-12.9396941466076,66.7025491386527,-47.6747576852225));
#38640=CARTESIAN_POINT('Ctrl Pts',(-12.8407204020393,66.8991702874115,-47.756660010524));
#38641=CARTESIAN_POINT('Ctrl Pts',(-12.6384034068036,67.3227889604638,-47.9589770057598));
#38642=CARTESIAN_POINT('Ctrl Pts',(-12.5274124834039,67.5720741794367,-48.0977834762384));
#38643=CARTESIAN_POINT('Ctrl Pts',(-12.4337567297464,67.8166247903887,-48.2599999999944));
#38644=CARTESIAN_POINT('Origin',(-6.66025403785042,70.5000000000327,-58.2599999999947));
#38645=CARTESIAN_POINT('Origin',(-9.54700538384715,64.4999999999613,-53.2599999999105));
#38646=CARTESIAN_POINT('Origin',(-18.000000000005,58.5000000000228,-137.259999999993));
#38647=CARTESIAN_POINT('',(-18.0000000000061,70.5000000000322,-53.2599999999947));
#38648=CARTESIAN_POINT('Ctrl Pts',(-18.000000000006,70.5000000000323,-53.2599999999947));
#38649=CARTESIAN_POINT('Ctrl Pts',(-19.086410996523,70.5000000000323,-52.4917914172019));
#38650=CARTESIAN_POINT('Ctrl Pts',(-20.2690911668356,70.3448922127468,-51.6543584472451));
#38651=CARTESIAN_POINT('Ctrl Pts',(-21.7859823179493,69.8933981532665,-50.6171991515149));
#38652=CARTESIAN_POINT('Ctrl Pts',(-22.1460577379839,69.7674744253008,-50.3739179910419));
#38653=CARTESIAN_POINT('Ctrl Pts',(-22.5000000000059,69.6242977306757,-50.138850729658));
#38654=CARTESIAN_POINT('Ctrl Pts',(-13.500000000006,69.6242977306764,-50.138850729658));
#38655=CARTESIAN_POINT('Ctrl Pts',(-13.853942262028,69.7674744253015,-50.3739179910419));
#38656=CARTESIAN_POINT('Ctrl Pts',(-14.2140176820627,69.8933981532672,-50.6171991515149));
#38657=CARTESIAN_POINT('Ctrl Pts',(-15.7309088331764,70.3448922127472,-51.6543584472451));
#38658=CARTESIAN_POINT('Ctrl Pts',(-16.9135890034891,70.5000000000324,-52.4917914172019));
#38659=CARTESIAN_POINT('Ctrl Pts',(-18.000000000006,70.5000000000323,-53.2599999999947));
#38660=CARTESIAN_POINT('',(-18.0000000000061,70.5000000000236,-131.259999999995));
#38661=CARTESIAN_POINT('Ctrl Pts',(-18.000000000006,70.5000000000236,-131.259999999995));
#38662=CARTESIAN_POINT('Ctrl Pts',(-16.9135890034891,70.5000000000236,-132.028208582787));
#38663=CARTESIAN_POINT('Ctrl Pts',(-15.7309088331765,70.3448922127382,-132.865641552744));
#38664=CARTESIAN_POINT('Ctrl Pts',(-14.2140176820627,69.8933981532579,-133.902800848474));
#38665=CARTESIAN_POINT('Ctrl Pts',(-13.8539422620281,69.7674744252922,-134.146082008947));
#38666=CARTESIAN_POINT('Ctrl Pts',(-13.5000000000062,69.6242977306671,-134.381149270331));
#38667=CARTESIAN_POINT('Ctrl Pts',(-22.5000000000058,69.6242977306663,-134.381149270331));
#38668=CARTESIAN_POINT('Ctrl Pts',(-22.1460577379839,69.7674744252914,-134.146082008947));
#38669=CARTESIAN_POINT('Ctrl Pts',(-21.7859823179493,69.8933981532572,-133.902800848474));
#38670=CARTESIAN_POINT('Ctrl Pts',(-20.2690911668356,70.3448922127378,-132.865641552744));
#38671=CARTESIAN_POINT('Ctrl Pts',(-19.086410996523,70.5000000000234,-132.028208582787));
#38672=CARTESIAN_POINT('Ctrl Pts',(-18.000000000006,70.5000000000236,-131.259999999995));
#38673=CARTESIAN_POINT('Origin',(-36.000000000005,58.5000000000212,-137.259999999993));
#38674=CARTESIAN_POINT('',(-36.000000000006,70.5000000000306,-53.2599999999948));
#38675=CARTESIAN_POINT('Ctrl Pts',(-36.000000000006,70.5000000000307,-53.2599999999947));
#38676=CARTESIAN_POINT('Ctrl Pts',(-37.086410996523,70.5000000000307,-52.4917914172019));
#38677=CARTESIAN_POINT('Ctrl Pts',(-38.2690911668355,70.3448922127453,-51.654358447245));
#38678=CARTESIAN_POINT('Ctrl Pts',(-39.7859823179492,69.8933981532649,-50.6171991515149));
#38679=CARTESIAN_POINT('Ctrl Pts',(-40.1460577379839,69.7674744252992,-50.3739179910419));
#38680=CARTESIAN_POINT('Ctrl Pts',(-40.5000000000059,69.6242977306741,-50.138850729658));
#38681=CARTESIAN_POINT('Ctrl Pts',(-31.5000000000061,69.6242977306749,-50.138850729658));
#38682=CARTESIAN_POINT('Ctrl Pts',(-31.8539422620281,69.7674744252999,-50.3739179910419));
#38683=CARTESIAN_POINT('Ctrl Pts',(-32.2140176820627,69.8933981532656,-50.6171991515149));
#38684=CARTESIAN_POINT('Ctrl Pts',(-33.7309088331765,70.3448922127456,-51.654358447245));
#38685=CARTESIAN_POINT('Ctrl Pts',(-34.9135890034891,70.5000000000309,-52.4917914172019));
#38686=CARTESIAN_POINT('Ctrl Pts',(-36.000000000006,70.5000000000307,-53.2599999999947));
#38687=CARTESIAN_POINT('',(-36.000000000006,70.500000000022,-131.259999999995));
#38688=CARTESIAN_POINT('Ctrl Pts',(-36.000000000006,70.500000000022,-131.259999999995));
#38689=CARTESIAN_POINT('Ctrl Pts',(-34.9135890034891,70.500000000022,-132.028208582787));
#38690=CARTESIAN_POINT('Ctrl Pts',(-33.7309088331766,70.3448922127366,-132.865641552744));
#38691=CARTESIAN_POINT('Ctrl Pts',(-32.2140176820628,69.8933981532563,-133.902800848474));
#38692=CARTESIAN_POINT('Ctrl Pts',(-31.8539422620281,69.7674744252905,-134.146082008947));
#38693=CARTESIAN_POINT('Ctrl Pts',(-31.5000000000061,69.6242977306655,-134.381149270331));
#38694=CARTESIAN_POINT('Ctrl Pts',(-40.5000000000058,69.6242977306647,-134.381149270331));
#38695=CARTESIAN_POINT('Ctrl Pts',(-40.1460577379838,69.7674744252898,-134.146082008947));
#38696=CARTESIAN_POINT('Ctrl Pts',(-39.7859823179492,69.8933981532556,-133.902800848474));
#38697=CARTESIAN_POINT('Ctrl Pts',(-38.2690911668355,70.3448922127362,-132.865641552744));
#38698=CARTESIAN_POINT('Ctrl Pts',(-37.086410996523,70.5000000000218,-132.028208582787));
#38699=CARTESIAN_POINT('Ctrl Pts',(-36.000000000006,70.500000000022,-131.259999999995));
#38700=CARTESIAN_POINT('Origin',(-54.000000000005,58.5000000000197,-137.259999999993));
#38701=CARTESIAN_POINT('',(-54.000000000006,70.5000000000204,-131.259999999995));
#38702=CARTESIAN_POINT('Ctrl Pts',(-54.0000000000061,70.5000000000204,-131.259999999995));
#38703=CARTESIAN_POINT('Ctrl Pts',(-52.9135890034891,70.5000000000204,-132.028208582787));
#38704=CARTESIAN_POINT('Ctrl Pts',(-51.7309088331764,70.344892212735,-132.865641552744));
#38705=CARTESIAN_POINT('Ctrl Pts',(-50.2140176820627,69.8933981532547,-133.902800848474));
#38706=CARTESIAN_POINT('Ctrl Pts',(-49.8539422620281,69.767474425289,-134.146082008947));
#38707=CARTESIAN_POINT('Ctrl Pts',(-49.5000000000061,69.624297730664,-134.381149270331));
#38708=CARTESIAN_POINT('',(-54.000000000006,70.5000000000292,-53.2599999999947));
#38709=CARTESIAN_POINT('',(-54.000000000006,70.5000000000197,-137.259999999995));
#38710=CARTESIAN_POINT('Ctrl Pts',(-49.500000000006,69.6242977306733,-50.1388507296581));
#38711=CARTESIAN_POINT('Ctrl Pts',(-49.853942262028,69.7674744252984,-50.373917991042));
#38712=CARTESIAN_POINT('Ctrl Pts',(-50.2140176820627,69.893398153264,-50.617199151515));
#38713=CARTESIAN_POINT('Ctrl Pts',(-51.7309088331764,70.3448922127441,-51.6543584472451));
#38714=CARTESIAN_POINT('Ctrl Pts',(-52.9135890034891,70.5000000000293,-52.4917914172019));
#38715=CARTESIAN_POINT('Ctrl Pts',(-54.0000000000061,70.5000000000291,-53.2599999999947));
#38716=CARTESIAN_POINT('Origin',(74.499999999994,70.5000000000309,-137.259999999995));
#38717=CARTESIAN_POINT('',(-74.500000000006,70.5000000000179,-137.259999999995));
#38718=CARTESIAN_POINT('',(74.499999999994,70.5000000000403,-53.2599999999947));
#38719=CARTESIAN_POINT('',(74.499999999994,70.5000000000316,-131.259999999995));
#38720=CARTESIAN_POINT('Origin',(-59.000000000006,70.5000000000293,-47.2599999999947));
#38721=CARTESIAN_POINT('',(-59.0000000000057,66.5000000000293,-47.6031457505019));
#38722=CARTESIAN_POINT('',(-59.0000000000057,66.5000000000286,-53.2599999999943));
#38723=CARTESIAN_POINT('Origin',(-59.0000000000055,64.5000000000287,-53.259999999994));
#38724=CARTESIAN_POINT('Ctrl Pts',(-73.0104689725931,67.9465182387393,-136.171365597276));
#38725=CARTESIAN_POINT('Ctrl Pts',(-73.8703570864329,67.3703570864452,-136.57568286515));
#38726=CARTESIAN_POINT('Ctrl Pts',(-74.4465182387269,66.5104689726054,-136.171365597276));
#38727=CARTESIAN_POINT('Ctrl Pts',(-72.7182901970741,67.4456403378437,-136.522853342713));
#38728=CARTESIAN_POINT('Ctrl Pts',(-73.4169322419492,66.9169322419576,-136.80863897917));
#38729=CARTESIAN_POINT('Ctrl Pts',(-73.9456403378363,66.2182901970746,-136.52285334271));
#38730=CARTESIAN_POINT('Ctrl Pts',(-72.3945521743876,66.8906608703868,-136.79707108069));
#38731=CARTESIAN_POINT('Ctrl Pts',(-72.9358474574371,66.4358474574396,-136.981577743066));
#38732=CARTESIAN_POINT('Ctrl Pts',(-73.3906608703737,65.8945521743998,-136.797071080691));
#38733=CARTESIAN_POINT('Ctrl Pts',(-71.7138256723184,65.7237011525547,-137.16567278462));
#38734=CARTESIAN_POINT('Ctrl Pts',(-71.9760256068087,65.476025606831,-137.204292118055));
#38735=CARTESIAN_POINT('Ctrl Pts',(-72.2237011525427,65.2138256723311,-137.16567278462));
#38736=CARTESIAN_POINT('Ctrl Pts',(-71.3569625715572,65.1119358369451,-137.259999999994));
#38737=CARTESIAN_POINT('Ctrl Pts',(-71.4844140292029,64.9844140291876,-137.259999999994));
#38738=CARTESIAN_POINT('Ctrl Pts',(-71.6119358369396,64.8569625715567,-137.259999999994));
#38739=CARTESIAN_POINT('Ctrl Pts',(-71.0000000000055,64.5000000000182,-137.259999999994));
#38740=CARTESIAN_POINT('Ctrl Pts',(-71.0000000000055,64.5000000000182,-137.259999999994));
#38741=CARTESIAN_POINT('Ctrl Pts',(-71.0000000000055,64.5000000000182,-137.259999999994));
#38742=CARTESIAN_POINT('',(-71.0000000000055,64.5000000000182,-137.259999999994));
#38743=CARTESIAN_POINT('',(-72.1666666648479,66.4999929738548,-136.916834384971));
#38744=CARTESIAN_POINT('Ctrl Pts',(-71.0000000000055,64.5000000000182,-137.259999999994));
#38745=CARTESIAN_POINT('Ctrl Pts',(-71.0461016235444,64.579031354654,-137.259999999994));
#38746=CARTESIAN_POINT('Ctrl Pts',(-71.0901862514509,64.6546050024919,-137.258430124937));
#38747=CARTESIAN_POINT('Ctrl Pts',(-71.1322321415784,64.7266836712807,-137.255691250101));
#38748=CARTESIAN_POINT('Ctrl Pts',(-71.1769086032859,64.8032718913493,-137.252781019485));
#38749=CARTESIAN_POINT('Ctrl Pts',(-71.2192833734128,64.8759143544232,-137.248551330288));
#38750=CARTESIAN_POINT('Ctrl Pts',(-71.2593483300541,64.9445971372364,-137.243432561143));
#38751=CARTESIAN_POINT('Ctrl Pts',(-71.3005720467883,65.0152663659233,-137.238165746776));
#38752=CARTESIAN_POINT('Ctrl Pts',(-71.3393520927811,65.0817464447679,-137.231957549005));
#38753=CARTESIAN_POINT('Ctrl Pts',(-71.3756897878606,65.1440396363329,-137.22522199684));
#38754=CARTESIAN_POINT('Ctrl Pts',(-71.4119624699439,65.2062213770471,-137.218498495478));
#38755=CARTESIAN_POINT('Ctrl Pts',(-71.4458000279303,65.2642286193098,-137.211249696265));
#38756=CARTESIAN_POINT('Ctrl Pts',(-71.4772099370766,65.3180741778466,-137.203835335352));
#38757=CARTESIAN_POINT('Ctrl Pts',(-71.4992812448217,65.35591070541,-137.198625366718));
#38758=CARTESIAN_POINT('Ctrl Pts',(-71.5201539937003,65.3916925606305,-137.193332564077));
#38759=CARTESIAN_POINT('Ctrl Pts',(-71.5398318905126,65.4254260980235,-137.18806669589));
#38760=CARTESIAN_POINT('Ctrl Pts',(-71.5490219770469,65.4411805320823,-137.185607399311));
#38761=CARTESIAN_POINT('Ctrl Pts',(-71.5579523745364,65.4564872937506,-137.183153944699));
#38762=CARTESIAN_POINT('Ctrl Pts',(-71.5666244905579,65.4713462493087,-137.180716763366));
#38763=CARTESIAN_POINT('Ctrl Pts',(-71.5709605485687,65.4787757270877,-137.1794981727));
#38764=CARTESIAN_POINT('Ctrl Pts',(-71.5752312809214,65.4860939885622,-137.178283521247));
#38765=CARTESIAN_POINT('Ctrl Pts',(-71.5794366876175,65.4933011826271,-137.177074024157));
#38766=CARTESIAN_POINT('Ctrl Pts',(-71.5815393909655,65.4969047796595,-137.176469275612));
#38767=CARTESIAN_POINT('Ctrl Pts',(-71.5836257628995,65.5004806097435,-137.1758658151));
#38768=CARTESIAN_POINT('Ctrl Pts',(-71.5856958034194,65.504028691868,-137.175263791));
#38769=CARTESIAN_POINT('Ctrl Pts',(-71.5867308236794,65.5058027329303,-137.174962778951));
#38770=CARTESIAN_POINT('Ctrl Pts',(-71.5877617610859,65.5075698369966,-137.17466212597));
#38771=CARTESIAN_POINT('Ctrl Pts',(-71.5887886156389,65.5093300064616,-137.174361850386));
#38772=CARTESIAN_POINT('Ctrl Pts',(-71.5898154701919,65.5110901759266,-137.174061574802));
#38773=CARTESIAN_POINT('Ctrl Pts',(-71.5901645498526,65.5116885240887,-137.173959747421));
#38774=CARTESIAN_POINT('Ctrl Pts',(-71.5918569307377,65.5145897134391,-137.173462174011));
#38775=CARTESIAN_POINT('Ctrl Pts',(-71.6518002518728,65.6173484519944,-137.15583836189));
#38776=CARTESIAN_POINT('Ctrl Pts',(-71.7098470458656,65.7168576128275,-137.136026817555));
#38777=CARTESIAN_POINT('Ctrl Pts',(-71.7659715645342,65.8130727552615,-137.11446823468));
#38778=CARTESIAN_POINT('Ctrl Pts',(-71.8241491395591,65.9128074844008,-137.092121030599));
#38779=CARTESIAN_POINT('Ctrl Pts',(-71.8802613524022,66.0090029944704,-137.067896759689));
#38780=CARTESIAN_POINT('Ctrl Pts',(-71.9343032167983,66.1016493462721,-137.0422526908));
#38781=CARTESIAN_POINT('Ctrl Pts',(-71.9754646443761,66.1722141971086,-137.022720676201));
#38782=CARTESIAN_POINT('Ctrl Pts',(-72.0154255326638,66.2407209632734,-137.002364302726));
#38783=CARTESIAN_POINT('Ctrl Pts',(-72.0541916345281,66.3071785462513,-136.981372711329));
#38784=CARTESIAN_POINT('Ctrl Pts',(-72.0928696558172,66.3734851307576,-136.960428814989));
#38785=CARTESIAN_POINT('Ctrl Pts',(-72.1303568121008,66.4377492555433,-136.938853587582));
#38786=CARTESIAN_POINT('Ctrl Pts',(-72.1666666648479,66.4999929738547,-136.916834384971));
#38787=CARTESIAN_POINT('',(-74.4285713480856,66.4999999931934,-136.183910712889));
#38788=CARTESIAN_POINT('Ctrl Pts',(-74.4285712620137,66.4999999864247,-136.183910589276));
#38789=CARTESIAN_POINT('Ctrl Pts',(-74.3391637351035,66.447846586649,-136.246162395812));
#38790=CARTESIAN_POINT('Ctrl Pts',(-74.2459677079227,66.3934823597197,-136.307411277845));
#38791=CARTESIAN_POINT('Ctrl Pts',(-74.1489208833848,66.3368715577722,-136.367216310645));
#38792=CARTESIAN_POINT('Ctrl Pts',(-74.0544352094021,66.2817547643873,-136.425443036336));
#38793=CARTESIAN_POINT('Ctrl Pts',(-73.9562991774979,66.2245083351006,-136.482301080738));
#38794=CARTESIAN_POINT('Ctrl Pts',(-73.8544881487993,66.1651183162972,-136.53735222905));
#38795=CARTESIAN_POINT('Ctrl Pts',(-73.7991624013817,66.1328448266622,-136.567267906806));
#38796=CARTESIAN_POINT('Ctrl Pts',(-73.7427520100897,66.0999386725625,-136.596649461807));
#38797=CARTESIAN_POINT('Ctrl Pts',(-73.685257471521,66.0664001917311,-136.625422584916));
#38798=CARTESIAN_POINT('Ctrl Pts',(-73.5833222371684,66.0069379716926,-136.676436039762));
#38799=CARTESIAN_POINT('Ctrl Pts',(-73.4779732706246,65.9454844078761,-136.725541064569));
#38800=CARTESIAN_POINT('Ctrl Pts',(-73.3692181586471,65.88204392589,-136.772307970056));
#38801=CARTESIAN_POINT('Ctrl Pts',(-73.2532698589162,65.8144074177144,-136.822168092274));
#38802=CARTESIAN_POINT('Ctrl Pts',(-73.1334511973744,65.7445131984825,-136.869370640943));
#38803=CARTESIAN_POINT('Ctrl Pts',(-73.0098028938484,65.6723850214261,-136.913354442426));
#38804=CARTESIAN_POINT('Ctrl Pts',(-72.943363784672,65.6336288744067,-136.936987961896));
#38805=CARTESIAN_POINT('Ctrl Pts',(-72.8758195815183,65.5942280892339,-136.959691412332));
#38806=CARTESIAN_POINT('Ctrl Pts',(-72.8071810114582,65.5541889233654,-136.981371932656));
#38807=CARTESIAN_POINT('Ctrl Pts',(-72.8062002761416,65.5536168277641,-136.981681712593));
#38808=CARTESIAN_POINT('Ctrl Pts',(-72.8052193178398,65.553044602088,-136.981991283528));
#38809=CARTESIAN_POINT('Ctrl Pts',(-72.8042381365472,65.552472246334,-136.982300645237));
#38810=CARTESIAN_POINT('Ctrl Pts',(-72.8017395376995,65.5510147303395,-136.983088441353));
#38811=CARTESIAN_POINT('Ctrl Pts',(-72.7982538835131,65.548981439413,-136.984184208637));
#38812=CARTESIAN_POINT('Ctrl Pts',(-72.7967379885939,65.5480971731278,-136.984659963736));
#38813=CARTESIAN_POINT('Ctrl Pts',(-72.7414940646765,65.5158717604272,-137.001997958729));
#38814=CARTESIAN_POINT('Ctrl Pts',(-72.6820631103128,65.4812037746268,-137.019769083906));
#38815=CARTESIAN_POINT('Ctrl Pts',(-72.6183862784162,65.4440589628055,-137.037593809158));
#38816=CARTESIAN_POINT('Ctrl Pts',(-72.5555242070729,65.4073894278867,-137.055190462715));
#38817=CARTESIAN_POINT('Ctrl Pts',(-72.488523722678,65.3683057566253,-137.072839273218));
#38818=CARTESIAN_POINT('Ctrl Pts',(-72.4173412109389,65.32678256416,-137.09012722741));
#38819=CARTESIAN_POINT('Ctrl Pts',(-72.3480489944229,65.2863620455178,-137.106956089383));
#38820=CARTESIAN_POINT('Ctrl Pts',(-72.2747934881158,65.2436296031994,-137.123442835596));
#38821=CARTESIAN_POINT('Ctrl Pts',(-72.1975535325183,65.1985729267082,-137.139162840554));
#38822=CARTESIAN_POINT('Ctrl Pts',(-72.1522112972097,65.1721232684726,-137.148390968125));
#38823=CARTESIAN_POINT('Ctrl Pts',(-72.1054963903019,65.1448728943557,-137.157354060421));
#38824=CARTESIAN_POINT('Ctrl Pts',(-72.0574086363209,65.1168217045333,-137.165959242809));
#38825=CARTESIAN_POINT('Ctrl Pts',(-71.9810177539599,65.0722603564892,-137.179629198693));
#38826=CARTESIAN_POINT('Ctrl Pts',(-71.9011695232922,65.0256822219329,-137.192396570263));
#38827=CARTESIAN_POINT('Ctrl Pts',(-71.8178491645093,64.9770786793099,-137.203866314643));
#38828=CARTESIAN_POINT('Ctrl Pts',(-71.7364284600082,64.9295832683514,-137.21507455572));
#38829=CARTESIAN_POINT('Ctrl Pts',(-71.6516918329836,64.8801535692547,-137.225043624773));
#38830=CARTESIAN_POINT('Ctrl Pts',(-71.56365242532,64.8287972481189,-137.233368196345));
#38831=CARTESIAN_POINT('Ctrl Pts',(-71.476167290577,64.7777642528534,-137.241640358608));
#38832=CARTESIAN_POINT('Ctrl Pts',(-71.3854204310927,64.7248285848223,-137.24828872839));
#38833=CARTESIAN_POINT('Ctrl Pts',(-71.2914570392138,64.6700166062268,-137.252878611791));
#38834=CARTESIAN_POINT('Ctrl Pts',(-71.1974936473348,64.6152046276313,-137.257468495192));
#38835=CARTESIAN_POINT('Ctrl Pts',(-71.1003132543675,64.5585160650665,-137.259999999994));
#38836=CARTESIAN_POINT('Ctrl Pts',(-71.0000000000055,64.5000000000182,-137.259999999994));
#38837=CARTESIAN_POINT('Ctrl Pts',(-74.4285712620158,66.5000000000181,-136.183910589275));
#38838=CARTESIAN_POINT('Ctrl Pts',(-74.0993880304178,66.5000000000181,-136.413114927177));
#38839=CARTESIAN_POINT('Ctrl Pts',(-73.7389828108934,66.500000000018,-136.595513985264));
#38840=CARTESIAN_POINT('Ctrl Pts',(-72.9737426228516,66.5000000000181,-136.848440511399));
#38841=CARTESIAN_POINT('Ctrl Pts',(-72.570991520028,66.5000000000181,-136.916795227754));
#38842=CARTESIAN_POINT('Ctrl Pts',(-72.1666666658345,66.5000000000182,-136.91683189978));
#38843=CARTESIAN_POINT('Origin',(74.499999999994,70.5000000000309,-137.259999999995));
#38844=CARTESIAN_POINT('',(74.499999999994,70.5000000000391,-63.2599999999947));
#38845=CARTESIAN_POINT('',(68.999999999994,70.5000000000387,-63.2599999999947));
#38846=CARTESIAN_POINT('',(68.999999999994,70.5000000000387,-63.2599999999947));
#38847=CARTESIAN_POINT('',(74.499999999994,70.5000000000327,-121.259999999995));
#38848=CARTESIAN_POINT('',(74.499999999994,70.5000000000309,-137.259999999995));
#38849=CARTESIAN_POINT('',(68.999999999994,70.5000000000323,-121.259999999995));
#38850=CARTESIAN_POINT('',(68.999999999994,70.5000000000322,-121.259999999995));
#38851=CARTESIAN_POINT('',(58.999999999994,70.5000000000303,-131.259999999995));
#38852=CARTESIAN_POINT('Origin',(68.999999999994,70.5000000000311,-131.259999999995));
#38853=CARTESIAN_POINT('',(74.499999999994,70.5000000000316,-131.259999999995));
#38854=CARTESIAN_POINT('',(58.999999999994,70.500000000039,-53.2599999999947));
#38855=CARTESIAN_POINT('',(74.499999999994,70.5000000000403,-53.2599999999947));
#38856=CARTESIAN_POINT('Origin',(68.999999999994,70.5000000000399,-53.2599999999947));
#38857=CARTESIAN_POINT('Origin',(58.999999999994,70.5000000000296,-137.259999999995));
#38858=CARTESIAN_POINT('',(58.9999999999943,66.5000000000296,-136.916854249486));
#38859=CARTESIAN_POINT('',(58.9999999999943,66.5000000000302,-131.259999999994));
#38860=CARTESIAN_POINT('',(58.9999999999943,66.5000000000302,-131.259999999994));
#38861=CARTESIAN_POINT('Origin',(58.9999999999945,64.5000000000302,-131.259999999994));
#38862=CARTESIAN_POINT('',(58.999999999994,70.5000000000302,-131.259999999995));
#38863=CARTESIAN_POINT('Origin',(68.999999999994,70.5000000000311,-131.259999999995));
#38864=CARTESIAN_POINT('',(68.9999999999943,66.5000000000322,-121.259999999994));
#38865=CARTESIAN_POINT('',(68.999999999994,70.5000000000322,-121.259999999995));
#38866=CARTESIAN_POINT('Origin',(68.9999999999943,66.5000000000311,-131.259999999994));
#38867=CARTESIAN_POINT('Origin',(68.999999999994,70.5000000000322,-121.259999999995));
#38868=CARTESIAN_POINT('',(76.9999999999942,68.0000000000328,-121.259999999994));
#38869=CARTESIAN_POINT('Origin',(74.4999999999942,68.0000000000327,-121.259999999994));
#38870=CARTESIAN_POINT('',(76.9999999999943,66.5000000000329,-121.259999999994));
#38871=CARTESIAN_POINT('',(76.999999999994,70.5000000000329,-121.259999999995));
#38872=CARTESIAN_POINT('',(68.9999999999943,66.5000000000322,-121.259999999994));
#38873=CARTESIAN_POINT('Origin',(74.4999999999945,64.5000000000316,-131.259999999994));
#38874=CARTESIAN_POINT('',(72.1666658662162,66.4999968842164,-136.916844121822));
#38875=CARTESIAN_POINT('',(68.9999999999943,66.5000000000304,-136.916854249486));
#38876=CARTESIAN_POINT('',(70.9999999999945,64.5000000000306,-137.259999999994));
#38877=CARTESIAN_POINT('Origin',(71.1254265028578,64.7149703218329,-132.635568492653));
#38878=CARTESIAN_POINT('',(74.4999999999945,64.5000000000309,-137.259999999994));
#38879=CARTESIAN_POINT('',(-69.0000000000057,66.5000000000185,-136.916854249486));
#38880=CARTESIAN_POINT('Origin',(63.2264973080965,85.77525231655,-131.259999999996));
#38881=CARTESIAN_POINT('',(63.2264973080981,66.5000000000306,-131.259999999994));
#38882=CARTESIAN_POINT('',(63.2264973080965,85.7752523165501,-131.259999999996));
#38883=CARTESIAN_POINT('',(66.1132486540463,66.5000000000314,-126.259999999994));
#38884=CARTESIAN_POINT('',(66.1132486540463,66.5000000000314,-126.259999999994));
#38885=CARTESIAN_POINT('',(66.1132486540445,85.7752523165508,-126.259999999996));
#38886=CARTESIAN_POINT('Origin',(66.1132486540445,85.7752523165498,-136.259999999996));
#38887=CARTESIAN_POINT('',(66.1132486540462,66.5000000000303,-136.259999999994));
#38888=CARTESIAN_POINT('',(66.1132486540445,85.7752523165498,-136.259999999996));
#38889=CARTESIAN_POINT('',(63.2264973080981,66.5000000000306,-131.259999999994));
#38890=CARTESIAN_POINT('Origin',(71.8867513459408,85.7752523165503,-136.259999999996));
#38891=CARTESIAN_POINT('',(71.8867513459424,66.5000000000308,-136.259999999994));
#38892=CARTESIAN_POINT('',(71.8867513459408,85.7752523165502,-136.259999999996));
#38893=CARTESIAN_POINT('',(68.9999999999943,66.5000000000305,-136.259999999994));
#38894=CARTESIAN_POINT('Origin',(74.773502691889,85.7752523165511,-131.259999999996));
#38895=CARTESIAN_POINT('',(74.7735026918906,66.5000000000316,-131.259999999994));
#38896=CARTESIAN_POINT('',(74.7735026918889,85.7752523165511,-131.259999999996));
#38897=CARTESIAN_POINT('',(71.8867513459424,66.5000000000308,-136.259999999994));
#38898=CARTESIAN_POINT('Origin',(71.8867513459408,85.7752523165513,-126.259999999996));
#38899=CARTESIAN_POINT('',(71.8867513459424,66.5000000000319,-126.259999999994));
#38900=CARTESIAN_POINT('',(71.8867513459408,85.7752523165513,-126.259999999996));
#38901=CARTESIAN_POINT('',(74.7735026918906,66.5000000000316,-131.259999999994));
#38902=CARTESIAN_POINT('Origin',(66.1132486540445,85.7752523165508,-126.259999999996));
#38903=CARTESIAN_POINT('',(68.9999999999943,66.5000000000316,-126.259999999994));
#38904=CARTESIAN_POINT('Ctrl Pts',(74.4465182387155,66.5104689726184,-136.171365597276));
#38905=CARTESIAN_POINT('Ctrl Pts',(73.8703570864215,67.3703570864582,-136.57568286515));
#38906=CARTESIAN_POINT('Ctrl Pts',(73.0104689725816,67.9465182387521,-136.171365597276));
#38907=CARTESIAN_POINT('Ctrl Pts',(73.9456403378197,66.2182901970983,-136.522853342714));
#38908=CARTESIAN_POINT('Ctrl Pts',(73.4169322419408,66.916932241965,-136.808638979169));
#38909=CARTESIAN_POINT('Ctrl Pts',(72.7182901970583,67.4456403378574,-136.522853342713));
#38910=CARTESIAN_POINT('Ctrl Pts',(73.3906608703643,65.8945521744123,-136.79707108069));
#38911=CARTESIAN_POINT('Ctrl Pts',(72.9358474574211,66.435847457458,-136.981577743062));
#38912=CARTESIAN_POINT('Ctrl Pts',(72.3945521743758,66.8906608704009,-136.79707108069));
#38913=CARTESIAN_POINT('Ctrl Pts',(72.2237011525298,65.2138256723439,-137.165672784621));
#38914=CARTESIAN_POINT('Ctrl Pts',(71.9760256068021,65.476025606838,-137.204292118059));
#38915=CARTESIAN_POINT('Ctrl Pts',(71.7138256723076,65.7237011525658,-137.165672784621));
#38916=CARTESIAN_POINT('Ctrl Pts',(71.6119358369269,64.8569625715743,-137.259999999994));
#38917=CARTESIAN_POINT('Ctrl Pts',(71.4844140291782,64.9844140292143,-137.259999999994));
#38918=CARTESIAN_POINT('Ctrl Pts',(71.3569625715387,65.1119358369628,-137.259999999994));
#38919=CARTESIAN_POINT('Ctrl Pts',(70.9999999999945,64.5000000000306,-137.259999999994));
#38920=CARTESIAN_POINT('Ctrl Pts',(70.9999999999945,64.5000000000306,-137.259999999994));
#38921=CARTESIAN_POINT('Ctrl Pts',(70.9999999999945,64.5000000000306,-137.259999999994));
#38922=CARTESIAN_POINT('',(74.4285713427324,66.5000000000331,-136.183910716608));
#38923=CARTESIAN_POINT('Ctrl Pts',(74.4285712566625,66.500000000031,-136.183910592995));
#38924=CARTESIAN_POINT('Ctrl Pts',(74.0993879142635,66.500000000031,-136.413115007304));
#38925=CARTESIAN_POINT('Ctrl Pts',(73.7389825693774,66.500000000031,-136.595514107423));
#38926=CARTESIAN_POINT('Ctrl Pts',(72.9737427869456,66.5000000000309,-136.848440414353));
#38927=CARTESIAN_POINT('Ctrl Pts',(72.5709914841384,66.5000000000308,-136.9167952487));
#38928=CARTESIAN_POINT('Ctrl Pts',(72.166666480424,66.5000000000307,-136.916831899798));
#38929=CARTESIAN_POINT('Ctrl Pts',(70.9999999999945,64.5000000000306,-137.259999999994));
#38930=CARTESIAN_POINT('Ctrl Pts',(71.0957024837609,64.5558264488943,-137.259999999994));
#38931=CARTESIAN_POINT('Ctrl Pts',(71.1885540281554,64.6099898497911,-137.257695594979));
#38932=CARTESIAN_POINT('Ctrl Pts',(71.2784807358408,64.662447095941,-137.253498369066));
#38933=CARTESIAN_POINT('Ctrl Pts',(71.3721446992566,64.7170844079336,-137.249126711029));
#38934=CARTESIAN_POINT('Ctrl Pts',(71.4626358478783,64.7698709112963,-137.242701781837));
#38935=CARTESIAN_POINT('Ctrl Pts',(71.5499081224735,64.8207797381435,-137.23465187225));
#38936=CARTESIAN_POINT('Ctrl Pts',(71.6395131549217,64.873049340405,-137.226386791352));
#38937=CARTESIAN_POINT('Ctrl Pts',(71.7257252428347,64.923339725021,-137.216408761768));
#38938=CARTESIAN_POINT('Ctrl Pts',(71.8085292801494,64.9716420801213,-137.205141858606));
#38939=CARTESIAN_POINT('Ctrl Pts',(71.8898271555678,65.019065840782,-137.194079894489));
#38940=CARTESIAN_POINT('Ctrl Pts',(71.9678403250929,65.064573523005,-137.181775307674));
#38941=CARTESIAN_POINT('Ctrl Pts',(72.0425811727914,65.1081723508292,-137.168593448589));
#38942=CARTESIAN_POINT('Ctrl Pts',(72.1076226249628,65.1461131979292,-137.157122247985));
#38943=CARTESIAN_POINT('Ctrl Pts',(72.1701809791262,65.1826055711912,-137.144986872136));
#38944=CARTESIAN_POINT('Ctrl Pts',(72.2302564698221,65.2176496074305,-137.132412503954));
#38945=CARTESIAN_POINT('Ctrl Pts',(72.3102097945727,65.2642890468684,-137.115677517171));
#38946=CARTESIAN_POINT('Ctrl Pts',(72.3857667799575,65.3083639550095,-137.098166525896));
#38947=CARTESIAN_POINT('Ctrl Pts',(72.4569627922973,65.3498949622077,-137.08036161178));
#38948=CARTESIAN_POINT('Ctrl Pts',(72.5277434635707,65.3911836871171,-137.062660567414));
#38949=CARTESIAN_POINT('Ctrl Pts',(72.5942132886545,65.4299577517494,-137.044669104252));
#38950=CARTESIAN_POINT('Ctrl Pts',(72.6564170382027,65.4662432723191,-137.026812358299));
#38951=CARTESIAN_POINT('Ctrl Pts',(72.7041780482294,65.4941038615013,-137.013101669977));
#38952=CARTESIAN_POINT('Ctrl Pts',(72.749424449516,65.5204975955851,-136.999469395453));
#38953=CARTESIAN_POINT('Ctrl Pts',(72.7921804221301,65.5454385796099,-136.986088323429));
#38954=CARTESIAN_POINT('Ctrl Pts',(72.7937027701776,65.5463266159709,-136.985611883587));
#38955=CARTESIAN_POINT('Ctrl Pts',(72.7942365687616,65.5466380145225,-136.985445020286));
#38956=CARTESIAN_POINT('Ctrl Pts',(72.7967379868563,65.548097175037,-136.984659964278));
#38957=CARTESIAN_POINT('Ctrl Pts',(72.8002217706516,65.5501293821942,-136.983566598318));
#38958=CARTESIAN_POINT('Ctrl Pts',(72.8037027766303,65.5521599690388,-136.982470585208));
#38959=CARTESIAN_POINT('Ctrl Pts',(72.8071810018965,65.5541889338815,-136.981371935672));
#38960=CARTESIAN_POINT('Ctrl Pts',(72.9237260583972,65.622173553661,-136.944559434345));
#38961=CARTESIAN_POINT('Ctrl Pts',(73.0371375340389,65.6883303450419,-136.90479193608));
#38962=CARTESIAN_POINT('Ctrl Pts',(73.1473464497032,65.752619050548,-136.862522044316));
#38963=CARTESIAN_POINT('Ctrl Pts',(73.2595780988789,65.8180876870811,-136.819476346656));
#38964=CARTESIAN_POINT('Ctrl Pts',(73.3684886881679,65.8816191152061,-136.773835536597));
#38965=CARTESIAN_POINT('Ctrl Pts',(73.4740420120092,65.943192153817,-136.726043991574));
#38966=CARTESIAN_POINT('Ctrl Pts',(73.5826686561035,66.0065579703311,-136.67686093449));
#38967=CARTESIAN_POINT('Ctrl Pts',(73.6877397828133,66.0678497509414,-136.625400110897));
#38968=CARTESIAN_POINT('Ctrl Pts',(73.7892526840887,66.1270658118495,-136.572110387094));
#38969=CARTESIAN_POINT('Ctrl Pts',(73.892600078187,66.1873519972184,-136.517857636773));
#38970=CARTESIAN_POINT('Ctrl Pts',(73.9922596634551,66.2454868689079,-136.461709251839));
#38971=CARTESIAN_POINT('Ctrl Pts',(74.0882638810283,66.3014892089543,-136.404102734114));
#38972=CARTESIAN_POINT('Ctrl Pts',(74.1868725239103,66.3590107938365,-136.344933453038));
#38973=CARTESIAN_POINT('Ctrl Pts',(74.2816249422558,66.414282667277,-136.284225864962));
#38974=CARTESIAN_POINT('Ctrl Pts',(74.3725906165779,66.4673451790332,-136.222416363546));
#38975=CARTESIAN_POINT('Ctrl Pts',(74.3914125813985,66.4783244933406,-136.209627184882));
#38976=CARTESIAN_POINT('Ctrl Pts',(74.4100725340541,66.4892092821663,-136.196790704302));
#38977=CARTESIAN_POINT('Ctrl Pts',(74.4285712566605,66.5000000000353,-136.183910592996));
#38978=CARTESIAN_POINT('Origin',(58.999999999994,70.5000000000397,-47.2599999999947));
#38979=CARTESIAN_POINT('',(58.9999999999943,66.5000000000389,-53.2599999999943));
#38980=CARTESIAN_POINT('',(58.999999999994,70.5000000000391,-53.2599999999947));
#38981=CARTESIAN_POINT('',(58.9999999999943,66.5000000000396,-47.6031457505019));
#38982=CARTESIAN_POINT('Origin',(58.9999999999945,64.5000000000389,-53.259999999994));
#38983=CARTESIAN_POINT('',(58.9999999999943,66.5000000000389,-53.2599999999943));
#38984=CARTESIAN_POINT('Origin',(68.999999999994,70.5000000000399,-53.2599999999947));
#38985=CARTESIAN_POINT('',(68.9999999999943,66.5000000000386,-63.2599999999943));
#38986=CARTESIAN_POINT('',(68.999999999994,70.5000000000387,-63.2599999999947));
#38987=CARTESIAN_POINT('Origin',(68.9999999999943,66.5000000000397,-53.2599999999943));
#38988=CARTESIAN_POINT('Origin',(68.999999999994,70.5000000000387,-63.2599999999947));
#38989=CARTESIAN_POINT('',(76.9999999999943,66.5000000000393,-63.2599999999942));
#38990=CARTESIAN_POINT('',(68.9999999999943,66.5000000000386,-63.2599999999942));
#38991=CARTESIAN_POINT('',(76.9999999999942,68.0000000000393,-63.2599999999944));
#38992=CARTESIAN_POINT('',(76.999999999994,70.5000000000394,-63.2599999999947));
#38993=CARTESIAN_POINT('Origin',(74.4999999999942,68.000000000039,-63.2599999999944));
#38994=CARTESIAN_POINT('Origin',(63.2264973080965,85.7752523165588,-53.2599999999964));
#38995=CARTESIAN_POINT('',(63.2264973080981,66.5000000000393,-53.2599999999942));
#38996=CARTESIAN_POINT('',(63.2264973080965,85.7752523165588,-53.2599999999965));
#38997=CARTESIAN_POINT('',(66.1132486540463,66.5000000000401,-48.2599999999942));
#38998=CARTESIAN_POINT('',(63.2264973080981,66.5000000000393,-53.2599999999943));
#38999=CARTESIAN_POINT('',(66.1132486540445,85.7752523165595,-48.2599999999964));
#39000=CARTESIAN_POINT('Origin',(66.1132486540445,85.7752523165595,-48.2599999999964));
#39001=CARTESIAN_POINT('',(71.8867513459424,66.5000000000406,-48.2599999999942));
#39002=CARTESIAN_POINT('',(68.9999999999943,66.5000000000403,-48.2599999999943));
#39003=CARTESIAN_POINT('',(71.8867513459408,85.77525231656,-48.2599999999964));
#39004=CARTESIAN_POINT('Origin',(71.8867513459408,85.77525231656,-48.2599999999964));
#39005=CARTESIAN_POINT('',(74.7735026918906,66.5000000000403,-53.2599999999943));
#39006=CARTESIAN_POINT('',(71.8867513459424,66.5000000000406,-48.2599999999943));
#39007=CARTESIAN_POINT('',(74.7735026918889,85.7752523165598,-53.2599999999965));
#39008=CARTESIAN_POINT('Origin',(74.773502691889,85.7752523165598,-53.2599999999964));
#39009=CARTESIAN_POINT('',(71.8867513459424,66.5000000000394,-58.2599999999942));
#39010=CARTESIAN_POINT('',(74.7735026918906,66.5000000000403,-53.2599999999943));
#39011=CARTESIAN_POINT('',(71.8867513459408,85.7752523165589,-58.2599999999964));
#39012=CARTESIAN_POINT('Origin',(71.8867513459408,85.7752523165589,-58.2599999999964));
#39013=CARTESIAN_POINT('',(66.1132486540463,66.5000000000389,-58.2599999999942));
#39014=CARTESIAN_POINT('',(68.9999999999943,66.5000000000392,-58.2599999999943));
#39015=CARTESIAN_POINT('',(66.1132486540446,85.7752523165584,-58.2599999999965));
#39016=CARTESIAN_POINT('Origin',(66.1132486540445,85.7752523165584,-58.2599999999964));
#39017=CARTESIAN_POINT('',(66.1132486540463,66.5000000000389,-58.2599999999943));
#39018=CARTESIAN_POINT('Origin',(88.6000000000047,-52.7216878364596,-62.9999999999805));
#39019=CARTESIAN_POINT('',(92.4000000000046,-50.5566243269593,-62.9999999999808));
#39020=CARTESIAN_POINT('',(88.6000000000045,-50.5566243269596,-62.9999999999808));
#39021=CARTESIAN_POINT('',(92.4000000000048,-53.4433756729593,-62.9999999999804));
#39022=CARTESIAN_POINT('',(88.6000000000048,-53.4433756729596,-62.9999999999804));
#39023=CARTESIAN_POINT('',(92.4000000000047,-51.9999999999593,-62.9999999999806));
#39024=CARTESIAN_POINT('Origin',(88.6000000000049,-54.1650635094095,-61.7499999999804));
#39025=CARTESIAN_POINT('',(92.4000000000049,-54.886751345859,-60.4999999999803));
#39026=CARTESIAN_POINT('',(88.6000000000049,-54.8867513458593,-60.4999999999803));
#39027=CARTESIAN_POINT('',(92.4000000000048,-53.4433756729593,-62.9999999999804));
#39028=CARTESIAN_POINT('Origin',(88.6000000000049,-54.1650635094092,-59.2499999999804));
#39029=CARTESIAN_POINT('',(92.4000000000048,-53.4433756729587,-57.9999999999804));
#39030=CARTESIAN_POINT('',(88.6000000000048,-53.4433756729591,-57.9999999999804));
#39031=CARTESIAN_POINT('',(92.4000000000049,-54.886751345859,-60.4999999999803));
#39032=CARTESIAN_POINT('Origin',(88.6000000000047,-51.999999999959,-57.9999999999806));
#39033=CARTESIAN_POINT('',(92.4000000000046,-50.5566243269587,-57.9999999999808));
#39034=CARTESIAN_POINT('',(88.6000000000045,-50.5566243269591,-57.9999999999808));
#39035=CARTESIAN_POINT('',(92.4000000000047,-51.9999999999587,-57.9999999999806));
#39036=CARTESIAN_POINT('Origin',(88.6000000000045,-49.8349364905092,-59.2499999999809));
#39037=CARTESIAN_POINT('',(92.4000000000045,-49.113248654059,-60.4999999999809));
#39038=CARTESIAN_POINT('',(88.6000000000044,-49.1132486540593,-60.4999999999809));
#39039=CARTESIAN_POINT('',(92.4000000000046,-50.5566243269587,-57.9999999999808));
#39040=CARTESIAN_POINT('Origin',(88.6000000000045,-49.8349364905095,-61.7499999999809));
#39041=CARTESIAN_POINT('',(92.4000000000045,-49.113248654059,-60.4999999999809));
#39042=CARTESIAN_POINT('Origin',(1.11022302462516E-13,3.94842578771426E-11,
-3.4999999999866));
#39043=CARTESIAN_POINT('Origin',(-95.1999999999911,-100.749999999987,-164.999999999975));
#39044=CARTESIAN_POINT('',(-95.199999999991,-102.193375672988,-167.499999999975));
#39045=CARTESIAN_POINT('',(-95.1999999999908,-103.636751345887,-164.999999999975));
#39046=CARTESIAN_POINT('',(-95.1999999999909,-102.915063509438,-166.249999999975));
#39047=CARTESIAN_POINT('',(-95.199999999991,-102.193375672987,-162.499999999975));
#39048=CARTESIAN_POINT('',(-95.1999999999909,-102.915063509437,-163.749999999975));
#39049=CARTESIAN_POINT('',(-95.1999999999912,-99.3066243269871,-162.499999999975));
#39050=CARTESIAN_POINT('',(-95.1999999999911,-100.749999999987,-162.499999999975));
#39051=CARTESIAN_POINT('',(-95.1999999999913,-97.8632486540874,-164.999999999976));
#39052=CARTESIAN_POINT('',(-95.1999999999913,-98.5849364905373,-163.749999999975));
#39053=CARTESIAN_POINT('',(-95.1999999999912,-99.3066243269877,-167.499999999975));
#39054=CARTESIAN_POINT('',(-95.1999999999913,-98.5849364905376,-166.249999999975));
#39055=CARTESIAN_POINT('',(-95.199999999991,-101.471687836488,-167.499999999975));
#39056=CARTESIAN_POINT('Origin',(-79.9999999999989,-11.1689999999897,-196.499999999986));
#39057=CARTESIAN_POINT('Origin',(1.74860126378462E-12,-18.7858057259555,
-153.999999999984));
#39058=CARTESIAN_POINT('',(74.5682819382939,71.0000000000287,-153.999999999995));
#39059=CARTESIAN_POINT('',(-74.5682819383061,71.0000000000157,-153.999999999995));
#39060=CARTESIAN_POINT('',(-6.07847105982273E-12,71.0000000000222,-153.999999999995));
#39061=CARTESIAN_POINT('',(76.9999999999951,59.5000000000279,-153.999999999993));
#39062=CARTESIAN_POINT('',(75.7841409691445,65.2500000000288,-153.999999999994));
#39063=CARTESIAN_POINT('',(74.6696035241941,69.0000000000287,-153.999999999995));
#39064=CARTESIAN_POINT('',(75.8348017620945,64.2500000000288,-153.999999999994));
#39065=CARTESIAN_POINT('',(-74.6696035242059,69.0000000000157,-153.999999999995));
#39066=CARTESIAN_POINT('',(-5.91193760612896E-12,69.0000000000222,-153.999999999995));
#39067=CARTESIAN_POINT('',(-77.0000000000051,59.5000000000154,-153.999999999993));
#39068=CARTESIAN_POINT('',(-75.8348017621055,64.2500000000156,-153.999999999994));
#39069=CARTESIAN_POINT('',(-75.7841409691556,65.2500000000156,-153.999999999994));
#39070=CARTESIAN_POINT('Origin',(-6.07847105982273E-12,71.0000000000233,
-143.999999999995));
#39071=CARTESIAN_POINT('',(-74.5682819383061,71.0000000000168,-143.999999999995));
#39072=CARTESIAN_POINT('',(74.5682819382939,71.0000000000298,-143.999999999995));
#39073=CARTESIAN_POINT('',(-6.07847105982273E-12,71.0000000000233,-143.999999999995));
#39074=CARTESIAN_POINT('',(74.5682819382939,71.0000000000298,-143.999999999995));
#39075=CARTESIAN_POINT('',(-74.5682819383061,71.0000000000168,-143.999999999995));
#39076=CARTESIAN_POINT('Origin',(1.74860126378462E-12,-18.7858057259544,
-143.999999999984));
#39077=CARTESIAN_POINT('',(77.0000000000095,59.4999999999543,-143.999999999993));
#39078=CARTESIAN_POINT('',(75.7841409691445,65.2500000000299,-143.999999999994));
#39079=CARTESIAN_POINT('',(-77.0000000000013,59.500000000037,-143.999999999993));
#39080=CARTESIAN_POINT('',(-75.7841409691556,65.2500000000167,-143.999999999994));
#39081=CARTESIAN_POINT('',(-74.6696035242059,69.0000000000168,-143.999999999994));
#39082=CARTESIAN_POINT('',(-75.8348017621055,64.2500000000167,-143.999999999994));
#39083=CARTESIAN_POINT('',(74.6696035241941,69.0000000000298,-143.999999999994));
#39084=CARTESIAN_POINT('',(-5.91193760612896E-12,69.0000000000233,-143.999999999994));
#39085=CARTESIAN_POINT('',(75.8348017620945,64.2500000000299,-143.999999999994));
#39086=CARTESIAN_POINT('Origin',(-5.91193760612896E-12,69.0000000000237,
-140.499999999994));
#39087=CARTESIAN_POINT('',(-74.6696035242059,69.0000000000172,-140.499999999994));
#39088=CARTESIAN_POINT('',(74.6696035241941,69.0000000000302,-140.499999999994));
#39089=CARTESIAN_POINT('',(-5.91193760612896E-12,69.0000000000237,-140.499999999994));
#39090=CARTESIAN_POINT('',(74.6696035241941,69.0000000000302,-140.499999999994));
#39091=CARTESIAN_POINT('',(-74.6696035242059,69.0000000000172,-140.499999999994));
#39092=CARTESIAN_POINT('Origin',(-68.5000000000024,28.778312163529,-43.2999999999899));
#39093=CARTESIAN_POINT('',(-68.5000000000023,28.056624327029,-43.4999999999899));
#39094=CARTESIAN_POINT('',(-68.5000000000023,28.056624327029,-43.2999999999898));
#39095=CARTESIAN_POINT('',(-68.5000000000026,30.943375673029,-43.4999999999902));
#39096=CARTESIAN_POINT('',(-68.5000000000026,30.943375673029,-43.2999999999901));
#39097=CARTESIAN_POINT('',(-68.5000000000025,29.5000000000289,-43.49999999999));
#39098=CARTESIAN_POINT('Origin',(-67.2500000000026,31.6650635094791,-43.2999999999902));
#39099=CARTESIAN_POINT('',(-66.0000000000027,32.3867513459292,-43.4999999999904));
#39100=CARTESIAN_POINT('',(-66.0000000000027,32.3867513459292,-43.2999999999903));
#39101=CARTESIAN_POINT('',(-68.5000000000026,30.943375673029,-43.4999999999902));
#39102=CARTESIAN_POINT('Origin',(-64.7500000000026,31.6650635094792,-43.2999999999902));
#39103=CARTESIAN_POINT('',(-63.5000000000026,30.9433756730294,-43.4999999999902));
#39104=CARTESIAN_POINT('',(-63.5000000000026,30.9433756730294,-43.2999999999901));
#39105=CARTESIAN_POINT('',(-66.0000000000027,32.3867513459292,-43.4999999999904));
#39106=CARTESIAN_POINT('Origin',(-63.5000000000025,29.5000000000294,-43.29999999999));
#39107=CARTESIAN_POINT('',(-63.5000000000023,28.0566243270294,-43.4999999999899));
#39108=CARTESIAN_POINT('',(-63.5000000000023,28.0566243270294,-43.2999999999898));
#39109=CARTESIAN_POINT('',(-63.5000000000025,29.5000000000294,-43.49999999999));
#39110=CARTESIAN_POINT('Origin',(-64.7500000000023,27.3349364905792,-43.2999999999898));
#39111=CARTESIAN_POINT('',(-66.0000000000022,26.6132486541292,-43.4999999999897));
#39112=CARTESIAN_POINT('',(-66.0000000000022,26.6132486541292,-43.2999999999896));
#39113=CARTESIAN_POINT('',(-63.5000000000023,28.0566243270294,-43.4999999999899));
#39114=CARTESIAN_POINT('Origin',(-67.2500000000023,27.3349364905791,-43.2999999999898));
#39115=CARTESIAN_POINT('',(-66.0000000000022,26.6132486541292,-43.4999999999897));
#39116=CARTESIAN_POINT('Origin',(84.2000000000047,-52.72168783646,-62.9999999999805));
#39117=CARTESIAN_POINT('',(84.4000000000048,-53.0627460667662,-62.9999999999805));
#39118=CARTESIAN_POINT('',(85.0000000000047,-52.4302858857085,-62.9999999999805));
#39119=CARTESIAN_POINT('Origin',(93.4000000000055,-60.9999999999592,-62.9999999999796));
#39120=CARTESIAN_POINT('',(84.4000000000048,-53.44337567296,-62.9999999999804));
#39121=CARTESIAN_POINT('',(84.4000000000047,-52.72168783646,-62.9999999999805));
#39122=CARTESIAN_POINT('',(84.2000000000048,-53.44337567296,-62.9999999999804));
#39123=CARTESIAN_POINT('',(85.0000000000045,-50.55662432696,-62.9999999999808));
#39124=CARTESIAN_POINT('',(84.2000000000046,-50.55662432696,-62.9999999999808));
#39125=CARTESIAN_POINT('',(85.0000000000052,-57.49999999996,-62.99999999998));
#39126=CARTESIAN_POINT('Origin',(84.2000000000045,-49.8349364905099,-61.7499999999809));
#39127=CARTESIAN_POINT('',(85.0000000000044,-49.1132486540597,-60.4999999999809));
#39128=CARTESIAN_POINT('',(84.2000000000044,-49.1132486540597,-60.4999999999809));
#39129=CARTESIAN_POINT('',(85.0000000000045,-50.55662432696,-62.9999999999808));
#39130=CARTESIAN_POINT('Origin',(84.2000000000045,-49.8349364905096,-59.2499999999809));
#39131=CARTESIAN_POINT('',(85.0000000000045,-50.5566243269594,-57.9999999999808));
#39132=CARTESIAN_POINT('',(84.2000000000046,-50.5566243269594,-57.9999999999808));
#39133=CARTESIAN_POINT('',(85.0000000000044,-49.1132486540597,-60.4999999999809));
#39134=CARTESIAN_POINT('Origin',(84.2000000000047,-51.9999999999594,-57.9999999999806));
#39135=CARTESIAN_POINT('',(84.4000000000048,-53.4433756729594,-57.9999999999804));
#39136=CARTESIAN_POINT('',(84.2000000000048,-53.4433756729594,-57.9999999999804));
#39137=CARTESIAN_POINT('',(84.4000000000048,-53.0627460667657,-57.9999999999805));
#39138=CARTESIAN_POINT('',(84.4000000000047,-51.9999999999594,-57.9999999999806));
#39139=CARTESIAN_POINT('',(85.0000000000047,-52.430285885708,-57.9999999999806));
#39140=CARTESIAN_POINT('Origin',(93.4000000000055,-60.9999999999586,-57.9999999999796));
#39141=CARTESIAN_POINT('',(85.0000000000052,-57.4999999999594,-57.99999999998));
#39142=CARTESIAN_POINT('Origin',(84.2000000000049,-54.1650635094096,-59.2499999999804));
#39143=CARTESIAN_POINT('',(84.4000000000049,-54.8867513458597,-60.4999999999803));
#39144=CARTESIAN_POINT('',(84.2000000000049,-54.8867513458597,-60.4999999999803));
#39145=CARTESIAN_POINT('',(84.4000000000048,-53.4433756729594,-57.9999999999804));
#39146=CARTESIAN_POINT('Origin',(84.2000000000049,-54.1650635094099,-61.7499999999804));
#39147=CARTESIAN_POINT('',(84.4000000000049,-54.8867513458597,-60.4999999999803));
#39148=CARTESIAN_POINT('Origin',(-92.4,2.17484450587558E-11,-87.4999999999866));
#39149=CARTESIAN_POINT('Origin',(-74.5000000000058,68.0000000000179,-137.259999999994));
#39150=CARTESIAN_POINT('',(-77.0000000000058,68.0000000000177,-137.259999999994));
#39151=CARTESIAN_POINT('Origin',(-69.0000000000057,66.5000000000191,-131.259999999994));
#39152=CARTESIAN_POINT('',(-77.0000000000057,66.5000000000183,-131.259999999994));
#39153=CARTESIAN_POINT('Origin',(-71.0000000000057,66.5000000000189,-131.259999999994));
#39154=CARTESIAN_POINT('',(-77.0000000000057,66.5000000000177,-137.259999999994));
#39155=CARTESIAN_POINT('Ctrl Pts',(-74.4465182387269,66.5104689726153,-48.3486344027126));
#39156=CARTESIAN_POINT('Ctrl Pts',(-73.8703570864329,67.3703570864552,-47.9443171348385));
#39157=CARTESIAN_POINT('Ctrl Pts',(-73.0104689725931,67.9465182387492,-48.3486344027127));
#39158=CARTESIAN_POINT('Ctrl Pts',(-73.9456403378346,66.2182901970878,-47.9971466572771));
#39159=CARTESIAN_POINT('Ctrl Pts',(-73.4169322419534,66.9169322419637,-47.7113610208082));
#39160=CARTESIAN_POINT('Ctrl Pts',(-72.718290197077,67.4456403378527,-47.9971466572743));
#39161=CARTESIAN_POINT('Ctrl Pts',(-73.3906608703745,65.8945521744096,-47.7229289192979));
#39162=CARTESIAN_POINT('Ctrl Pts',(-72.9358474574371,66.4358474574548,-47.5384222569253));
#39163=CARTESIAN_POINT('Ctrl Pts',(-72.3945521743876,66.8906608703965,-47.7229289192978));
#39164=CARTESIAN_POINT('Ctrl Pts',(-72.2237011525419,65.2138256723413,-47.3543272153676));
#39165=CARTESIAN_POINT('Ctrl Pts',(-71.9760256068088,65.476025606836,-47.3157078819302));
#39166=CARTESIAN_POINT('Ctrl Pts',(-71.7138256723184,65.7237011525651,-47.3543272153679));
#39167=CARTESIAN_POINT('Ctrl Pts',(-71.6119358369362,64.8569625715737,-47.2599999999941));
#39168=CARTESIAN_POINT('Ctrl Pts',(-71.4844140291975,64.984414029207,-47.2599999999941));
#39169=CARTESIAN_POINT('Ctrl Pts',(-71.3569625715513,65.1119358369585,-47.2599999999941));
#39170=CARTESIAN_POINT('Ctrl Pts',(-71.0000000000055,64.5000000000283,-47.259999999994));
#39171=CARTESIAN_POINT('Ctrl Pts',(-71.0000000000055,64.5000000000283,-47.259999999994));
#39172=CARTESIAN_POINT('Ctrl Pts',(-71.0000000000055,64.5000000000283,-47.259999999994));
#39173=CARTESIAN_POINT('',(-74.4285713427437,66.50000000003,-48.3360892833802));
#39174=CARTESIAN_POINT('',(-72.1666664804358,66.5000000000282,-47.603168100191));
#39175=CARTESIAN_POINT('Ctrl Pts',(-74.4285712566737,66.5000000000279,-48.336089406994));
#39176=CARTESIAN_POINT('Ctrl Pts',(-74.099387914276,66.5000000000279,-48.1068849926858));
#39177=CARTESIAN_POINT('Ctrl Pts',(-73.7389825693898,66.500000000028,-47.9244858925642));
#39178=CARTESIAN_POINT('Ctrl Pts',(-72.9737427869555,66.5000000000281,-47.6715595856325));
#39179=CARTESIAN_POINT('Ctrl Pts',(-72.5709914841508,66.5000000000281,-47.6032047512884));
#39180=CARTESIAN_POINT('Ctrl Pts',(-72.1666664804358,66.5000000000282,-47.603168100191));
#39181=CARTESIAN_POINT('',(-71.0000000000055,64.5000000000283,-47.259999999994));
#39182=CARTESIAN_POINT('Ctrl Pts',(-71.0000000000055,64.5000000000283,-47.259999999994));
#39183=CARTESIAN_POINT('Ctrl Pts',(-71.0957024839778,64.5558264490125,-47.259999999994));
#39184=CARTESIAN_POINT('Ctrl Pts',(-71.1885540285871,64.6099898500349,-47.2623044050192));
#39185=CARTESIAN_POINT('Ctrl Pts',(-71.278480736496,64.6624470963152,-47.2665016309523));
#39186=CARTESIAN_POINT('Ctrl Pts',(-71.3721447001262,64.7170844084331,-47.270873289009));
#39187=CARTESIAN_POINT('Ctrl Pts',(-71.4626358489729,64.769870911927,-47.2772982182316));
#39188=CARTESIAN_POINT('Ctrl Pts',(-71.5499081238032,64.8207797389114,-47.2853481278595));
#39189=CARTESIAN_POINT('Ctrl Pts',(-71.6395131564995,64.8730493413176,-47.2936132088008));
#39190=CARTESIAN_POINT('Ctrl Pts',(-71.7257252446709,64.9233397260842,-47.3035912384393));
#39191=CARTESIAN_POINT('Ctrl Pts',(-71.8085292822539,64.9716420813409,-47.3148581416667));
#39192=CARTESIAN_POINT('Ctrl Pts',(-71.8898271580062,65.0190658421964,-47.3259201058587));
#39193=CARTESIAN_POINT('Ctrl Pts',(-71.9678403278692,65.0645735246163,-47.3382246927615));
#39194=CARTESIAN_POINT('Ctrl Pts',(-72.0425811759093,65.1081723526396,-47.3514065519475));
#39195=CARTESIAN_POINT('Ctrl Pts',(-72.1076226269018,65.1461131990518,-47.3628777523782));
#39196=CARTESIAN_POINT('Ctrl Pts',(-72.1701809800006,65.1826055716927,-47.3750131280339));
#39197=CARTESIAN_POINT('Ctrl Pts',(-72.2302564697472,65.2176496073781,-47.3875874960164));
#39198=CARTESIAN_POINT('Ctrl Pts',(-72.3102097951455,65.2642890471937,-47.4043224829341));
#39199=CARTESIAN_POINT('Ctrl Pts',(-72.3857667811711,65.3083639557085,-47.4218334743689));
#39200=CARTESIAN_POINT('Ctrl Pts',(-72.4569627941448,65.3498949632764,-47.4396383886675));
#39201=CARTESIAN_POINT('Ctrl Pts',(-72.5277434860066,65.3911837001956,-47.4573394382061));
#39202=CARTESIAN_POINT('Ctrl Pts',(-72.59421332924,65.4299577754151,-47.4753309067242));
#39203=CARTESIAN_POINT('Ctrl Pts',(-72.6564170945389,65.4662433051727,-47.4931876578589));
#39204=CARTESIAN_POINT('Ctrl Pts',(-72.7041780837353,65.4941038822038,-47.5068983407079));
#39205=CARTESIAN_POINT('Ctrl Pts',(-72.7494244662453,65.5204976053346,-47.5205306097676));
#39206=CARTESIAN_POINT('Ctrl Pts',(-72.7921804221062,65.5454385795868,-47.5339116765479));
#39207=CARTESIAN_POINT('Ctrl Pts',(-72.7937027701653,65.5463266159546,-47.5343881163943));
#39208=CARTESIAN_POINT('Ctrl Pts',(-72.7942365687792,65.5466380145231,-47.5345549797046));
#39209=CARTESIAN_POINT('Ctrl Pts',(-72.7967379868677,65.548097175034,-47.5353400357101));
#39210=CARTESIAN_POINT('Ctrl Pts',(-72.8002217706629,65.5501293821912,-47.5364334016704));
#39211=CARTESIAN_POINT('Ctrl Pts',(-72.8037027766417,65.5521599690358,-47.5375294147803));
#39212=CARTESIAN_POINT('Ctrl Pts',(-72.807181001908,65.5541889338785,-47.5386280643162));
#39213=CARTESIAN_POINT('Ctrl Pts',(-72.9237260589525,65.6221735539754,-47.5754405658148));
#39214=CARTESIAN_POINT('Ctrl Pts',(-73.0371375351493,65.68833034568,-47.6152080642929));
#39215=CARTESIAN_POINT('Ctrl Pts',(-73.1473464513777,65.7526190515151,-47.6574779563107));
#39216=CARTESIAN_POINT('Ctrl Pts',(-73.2595781011115,65.8180876883735,-47.7005236542232));
#39217=CARTESIAN_POINT('Ctrl Pts',(-73.3684886909689,65.8816191168299,-47.7461644645764));
#39218=CARTESIAN_POINT('Ctrl Pts',(-73.4740420153865,65.9431921557768,-47.7939560099388));
#39219=CARTESIAN_POINT('Ctrl Pts',(-73.5826686600627,66.0065579726303,-47.8431390673672));
#39220=CARTESIAN_POINT('Ctrl Pts',(-73.6877397873635,66.0678497535853,-47.8945998913498));
#39221=CARTESIAN_POINT('Ctrl Pts',(-73.7892526892365,66.1270658148421,-47.9478896155913));
#39222=CARTESIAN_POINT('Ctrl Pts',(-73.892600083934,66.1873520005605,-48.002142366354));
#39223=CARTESIAN_POINT('Ctrl Pts',(-73.9922596698087,66.2454868726039,-48.0582907517788));
#39224=CARTESIAN_POINT('Ctrl Pts',(-74.088263887993,66.3014892130069,-48.1158972700473));
#39225=CARTESIAN_POINT('Ctrl Pts',(-74.1868725314681,66.3590107982352,-48.1750665516603));
#39226=CARTESIAN_POINT('Ctrl Pts',(-74.2816249504143,66.4142826720263,-48.2357741403271));
#39227=CARTESIAN_POINT('Ctrl Pts',(-74.3725906253415,66.4673451841354,-48.2975836423898));
#39228=CARTESIAN_POINT('Ctrl Pts',(-74.3914125871913,66.4783244967099,-48.3103728190844));
#39229=CARTESIAN_POINT('Ctrl Pts',(-74.4100725369295,66.4892092838339,-48.3232092976808));
#39230=CARTESIAN_POINT('Ctrl Pts',(-74.4285712566717,66.5000000000321,-48.3360894069926));
#39231=CARTESIAN_POINT('Origin',(-71.1248546100925,64.7150556883937,-51.8728787160349));
#39232=CARTESIAN_POINT('Origin',(-69.0000000000057,66.5000000000278,-53.2599999999943));
#39233=CARTESIAN_POINT('',(74.4999999999943,66.5000000000409,-47.6031457505019));
#39234=CARTESIAN_POINT('',(-77.0000000000057,66.5000000000271,-53.2599999999943));
#39235=CARTESIAN_POINT('',(-77.0000000000057,66.5000000000174,-137.259999999994));
#39236=CARTESIAN_POINT('Origin',(-71.0000000000057,66.5000000000276,-53.2599999999943));
#39237=CARTESIAN_POINT('Origin',(74.4999999999945,64.5000000000403,-53.259999999994));
#39238=CARTESIAN_POINT('',(70.9999999999945,64.5000000000407,-47.259999999994));
#39239=CARTESIAN_POINT('',(74.4999999999945,64.500000000041,-47.259999999994));
#39240=CARTESIAN_POINT('',(72.1666666657488,66.4999964869591,-47.6031556827593));
#39241=CARTESIAN_POINT('Origin',(71.1254680349722,64.7151828220995,-51.8829521166587));
#39242=CARTESIAN_POINT('',(68.9999999999943,66.5000000000404,-47.6031457505019));
#39243=CARTESIAN_POINT('Ctrl Pts',(73.0104689725816,67.9465182387619,-48.3486344027127));
#39244=CARTESIAN_POINT('Ctrl Pts',(73.8703570864216,67.3703570864681,-47.9443171348386));
#39245=CARTESIAN_POINT('Ctrl Pts',(74.4465182387155,66.5104689726283,-48.3486344027126));
#39246=CARTESIAN_POINT('Ctrl Pts',(72.7182901970595,67.4456403378679,-47.9971466572761));
#39247=CARTESIAN_POINT('Ctrl Pts',(73.4169322419358,66.9169322419847,-47.7113610208115));
#39248=CARTESIAN_POINT('Ctrl Pts',(73.9456403378217,66.2182901971061,-47.9971466572759));
#39249=CARTESIAN_POINT('Ctrl Pts',(72.3945521743758,66.8906608704091,-47.7229289192979));
#39250=CARTESIAN_POINT('Ctrl Pts',(72.935847457421,66.4358474574675,-47.5384222569253));
#39251=CARTESIAN_POINT('Ctrl Pts',(73.3906608703627,65.8945521744223,-47.7229289192977));
#39252=CARTESIAN_POINT('Ctrl Pts',(71.7138256723076,65.7237011525775,-47.3543272153679));
#39253=CARTESIAN_POINT('Ctrl Pts',(71.9760256068023,65.4760256068485,-47.3157078819302));
#39254=CARTESIAN_POINT('Ctrl Pts',(72.2237011525313,65.213825672354,-47.3543272153678));
#39255=CARTESIAN_POINT('Ctrl Pts',(71.356962571538,65.1119358369719,-47.2599999999941));
#39256=CARTESIAN_POINT('Ctrl Pts',(71.484414029178,64.9844140292242,-47.2599999999941));
#39257=CARTESIAN_POINT('Ctrl Pts',(71.611935836926,64.8569625715837,-47.2599999999941));
#39258=CARTESIAN_POINT('Ctrl Pts',(70.9999999999945,64.5000000000407,-47.259999999994));
#39259=CARTESIAN_POINT('Ctrl Pts',(70.9999999999945,64.5000000000407,-47.259999999994));
#39260=CARTESIAN_POINT('Ctrl Pts',(70.9999999999945,64.5000000000407,-47.259999999994));
#39261=CARTESIAN_POINT('',(74.4285713480745,66.4999999932162,-48.3360892871001));
#39262=CARTESIAN_POINT('Ctrl Pts',(74.4285712620025,66.4999999864476,-48.3360894107125));
#39263=CARTESIAN_POINT('Ctrl Pts',(74.3391637338871,66.4478465859688,-48.2738376033375));
#39264=CARTESIAN_POINT('Ctrl Pts',(74.2459677055059,66.3934823583403,-48.2125887205665));
#39265=CARTESIAN_POINT('Ctrl Pts',(74.1489208797793,66.3368715557003,-48.1527836871288));
#39266=CARTESIAN_POINT('Ctrl Pts',(74.0544352045465,66.2817547615872,-48.0945569607586));
#39267=CARTESIAN_POINT('Ctrl Pts',(73.956299171396,66.2245083315743,-48.037698915775));
#39268=CARTESIAN_POINT('Ctrl Pts',(73.8544881414612,66.1651183120502,-47.9826477669765));
#39269=CARTESIAN_POINT('Ctrl Pts',(73.7991623958305,66.1328448234576,-47.9527320902855));
#39270=CARTESIAN_POINT('Ctrl Pts',(73.7427520064248,66.0999386704583,-47.9233505363308));
#39271=CARTESIAN_POINT('Ctrl Pts',(73.6852574698426,66.0664001907854,-47.8945774142381));
#39272=CARTESIAN_POINT('Ctrl Pts',(73.5833222344415,66.0069379701348,-47.8435639589066));
#39273=CARTESIAN_POINT('Ctrl Pts',(73.4779732668583,65.9454844057112,-47.7944589336936));
#39274=CARTESIAN_POINT('Ctrl Pts',(73.3692181538548,65.8820439231259,-47.7476920278763));
#39275=CARTESIAN_POINT('Ctrl Pts',(73.253269855067,65.8144074154997,-47.6978319061833));
#39276=CARTESIAN_POINT('Ctrl Pts',(73.1334511946194,65.7445131969053,-47.650629358033));
#39277=CARTESIAN_POINT('Ctrl Pts',(73.0098028923415,65.6723850205766,-47.6066455570301));
#39278=CARTESIAN_POINT('Ctrl Pts',(72.9433637836261,65.633628873826,-47.5830120377442));
#39279=CARTESIAN_POINT('Ctrl Pts',(72.8758195809709,65.5942280889438,-47.5603085874872));
#39280=CARTESIAN_POINT('Ctrl Pts',(72.807181011447,65.5541889233882,-47.5386280673328));
#39281=CARTESIAN_POINT('Ctrl Pts',(72.8062002761214,65.5536168277816,-47.5383182873921));
#39282=CARTESIAN_POINT('Ctrl Pts',(72.8052193178106,65.5530446021003,-47.5380087164549));
#39283=CARTESIAN_POINT('Ctrl Pts',(72.8042381365091,65.552472246341,-47.5376993547426));
#39284=CARTESIAN_POINT('Ctrl Pts',(72.8017395376703,65.5510147303518,-47.53691155863));
#39285=CARTESIAN_POINT('Ctrl Pts',(72.7982538835186,65.548981439446,-47.5358157913566));
#39286=CARTESIAN_POINT('Ctrl Pts',(72.7967379885827,65.5480971731505,-47.5353400362519));
#39287=CARTESIAN_POINT('Ctrl Pts',(72.7414940634015,65.5158717596956,-47.5180020408631));
#39288=CARTESIAN_POINT('Ctrl Pts',(72.6820631077528,65.4812037731397,-47.5002309153228));
#39289=CARTESIAN_POINT('Ctrl Pts',(72.6183862745531,65.4440589605577,-47.4824061897516));
#39290=CARTESIAN_POINT('Ctrl Pts',(72.5555242019548,65.4073894249063,-47.4648095358888));
#39291=CARTESIAN_POINT('Ctrl Pts',(72.4885237162915,65.3683057529095,-47.4471607251225));
#39292=CARTESIAN_POINT('Ctrl Pts',(72.4173412032736,65.3267825597032,-47.4298727707195));
#39293=CARTESIAN_POINT('Ctrl Pts',(72.3480489855588,65.2863620403667,-47.4130439085518));
#39294=CARTESIAN_POINT('Ctrl Pts',(72.2747934780487,65.2436295973518,-47.3965571621923));
#39295=CARTESIAN_POINT('Ctrl Pts',(72.197553521247,65.1985729201613,-47.3808371571426));
#39296=CARTESIAN_POINT('Ctrl Pts',(72.152211288388,65.1721232633565,-47.3716090301599));
#39297=CARTESIAN_POINT('Ctrl Pts',(72.1054963841207,65.144872890781,-47.3626459384347));
#39298=CARTESIAN_POINT('Ctrl Pts',(72.0574086329714,65.1168217026105,-47.3540407565818));
#39299=CARTESIAN_POINT('Ctrl Pts',(71.9810177499806,65.0722603541992,-47.3403708006298));
#39300=CARTESIAN_POINT('Ctrl Pts',(71.9011695186989,65.0256822192849,-47.327603429021));
#39301=CARTESIAN_POINT('Ctrl Pts',(71.817849159319,64.9770786763137,-47.3161336846326));
#39302=CARTESIAN_POINT('Ctrl Pts',(71.7364284542443,64.9295832650206,-47.3049254435486));
#39303=CARTESIAN_POINT('Ctrl Pts',(71.6516918266631,64.8801535655991,-47.2949563745174));
#39304=CARTESIAN_POINT('Ctrl Pts',(71.5636524184613,64.828797244149,-47.2866318029957));
#39305=CARTESIAN_POINT('Ctrl Pts',(71.4761672846119,64.7777642494044,-47.2783596409185));
#39306=CARTESIAN_POINT('Ctrl Pts',(71.3854204261458,64.7248285819669,-47.271711271297));
#39307=CARTESIAN_POINT('Ctrl Pts',(71.2914570354089,64.6700166040371,-47.2671213880119));
#39308=CARTESIAN_POINT('Ctrl Pts',(71.197493644672,64.6152046261073,-47.2625315047268));
#39309=CARTESIAN_POINT('Ctrl Pts',(71.1003132529705,64.5585160642805,-47.259999999994));
#39310=CARTESIAN_POINT('Ctrl Pts',(70.9999999999945,64.5000000000407,-47.259999999994));
#39311=CARTESIAN_POINT('Ctrl Pts',(74.4285712620046,66.5000000000409,-48.3360894107137));
#39312=CARTESIAN_POINT('Ctrl Pts',(74.0993880304052,66.5000000000409,-48.1068850728108));
#39313=CARTESIAN_POINT('Ctrl Pts',(73.7389828108834,66.5000000000408,-47.9244860147235));
#39314=CARTESIAN_POINT('Ctrl Pts',(72.9737426228402,66.5000000000408,-47.6715594885888));
#39315=CARTESIAN_POINT('Ctrl Pts',(72.5709915200155,66.5000000000408,-47.6032047722343));
#39316=CARTESIAN_POINT('Ctrl Pts',(72.166666665823,66.5000000000407,-47.6031681002079));
#39317=CARTESIAN_POINT('Origin',(1.83186799063151E-12,-19.6933104181538,
-140.499999999984));
#39318=CARTESIAN_POINT('',(76.9999999999949,59.5000000000303,-140.499999999993));
#39319=CARTESIAN_POINT('',(75.8348017620945,64.2500000000304,-140.499999999994));
#39320=CARTESIAN_POINT('',(-77.0000000000051,59.5000000000171,-140.499999999993));
#39321=CARTESIAN_POINT('',(-75.8348017621055,64.2500000000171,-140.499999999994));
#39322=CARTESIAN_POINT('',(-5.07927033766009E-12,59.5000000000237,-140.499999999993));
#39323=CARTESIAN_POINT('Origin',(-71.0000000000058,68.0000000000186,-131.259999999994));
#39324=CARTESIAN_POINT('',(-77.000000000005,59.5000000000182,-131.259999999993));
#39325=CARTESIAN_POINT('',(-71.0000000000051,59.500000000018,-137.259999999993));
#39326=CARTESIAN_POINT('Origin',(-71.0000000000051,59.5000000000188,-131.259999999993));
#39327=CARTESIAN_POINT('',(-77.0000000000058,68.0000000000184,-131.259999999994));
#39328=CARTESIAN_POINT('',(-71.0000000000058,68.0000000000182,-137.259999999994));
#39329=CARTESIAN_POINT('Origin',(74.4999999999942,68.0000000000309,-137.259999999994));
#39330=CARTESIAN_POINT('',(70.9999999999949,59.5000000000305,-137.259999999993));
#39331=CARTESIAN_POINT('',(-5.07927033766009E-12,59.5000000000241,-137.259999999993));
#39332=CARTESIAN_POINT('',(70.9999999999942,68.0000000000307,-137.259999999994));
#39333=CARTESIAN_POINT('Origin',(74.4999999999942,68.0000000000309,-137.259999999994));
#39334=CARTESIAN_POINT('',(76.9999999999942,68.0000000000308,-137.259999999994));
#39335=CARTESIAN_POINT('Origin',(68.9999999999943,66.5000000000311,-131.259999999994));
#39336=CARTESIAN_POINT('',(76.9999999999943,66.5000000000318,-131.259999999994));
#39337=CARTESIAN_POINT('',(76.9999999999943,66.5000000000311,-137.259999999994));
#39338=CARTESIAN_POINT('Origin',(70.9999999999943,66.5000000000313,-131.259999999994));
#39339=CARTESIAN_POINT('Origin',(70.9999999999942,68.0000000000313,-131.259999999994));
#39340=CARTESIAN_POINT('',(76.9999999999949,59.5000000000317,-131.259999999993));
#39341=CARTESIAN_POINT('Origin',(70.9999999999949,59.5000000000313,-131.259999999993));
#39342=CARTESIAN_POINT('',(76.9999999999949,59.5000000000318,-131.259999999993));
#39343=CARTESIAN_POINT('Origin',(68.9999999999943,66.5000000000398,-53.2599999999943));
#39344=CARTESIAN_POINT('',(76.9999999999943,66.5000000000405,-53.2599999999942));
#39345=CARTESIAN_POINT('Origin',(70.9999999999944,66.50000000004,-53.2599999999942));
#39346=CARTESIAN_POINT('',(76.9999999999943,66.5000000000308,-137.259999999994));
#39347=CARTESIAN_POINT('Origin',(92.4000000000047,-51.999999999959,-60.4999999999806));
#39348=CARTESIAN_POINT('Origin',(-99.199999999991,-101.471687836488,-167.499999999975));
#39349=CARTESIAN_POINT('',(-98.999999999991,-102.193375672988,-167.499999999975));
#39350=CARTESIAN_POINT('',(-99.199999999991,-102.193375672988,-167.499999999975));
#39351=CARTESIAN_POINT('',(-98.9999999999912,-99.306624326988,-167.499999999975));
#39352=CARTESIAN_POINT('',(-99.1999999999912,-99.3066243269881,-167.499999999975));
#39353=CARTESIAN_POINT('',(-98.9999999999911,-100.749999999988,-167.499999999975));
#39354=CARTESIAN_POINT('Origin',(-99.1999999999913,-98.5849364905379,-166.249999999975));
#39355=CARTESIAN_POINT('',(-98.9999999999913,-97.8632486540878,-164.999999999976));
#39356=CARTESIAN_POINT('',(-99.1999999999914,-97.8632486540878,-164.999999999976));
#39357=CARTESIAN_POINT('',(-98.9999999999912,-99.306624326988,-167.499999999975));
#39358=CARTESIAN_POINT('Origin',(-99.1999999999913,-98.5849364905376,-163.749999999975));
#39359=CARTESIAN_POINT('',(-98.9999999999912,-99.3066243269875,-162.499999999975));
#39360=CARTESIAN_POINT('',(-99.1999999999912,-99.3066243269875,-162.499999999975));
#39361=CARTESIAN_POINT('',(-98.9999999999913,-97.8632486540878,-164.999999999976));
#39362=CARTESIAN_POINT('Origin',(-99.1999999999911,-100.749999999987,-162.499999999975));
#39363=CARTESIAN_POINT('',(-98.999999999991,-102.193375672987,-162.499999999975));
#39364=CARTESIAN_POINT('',(-99.199999999991,-102.193375672987,-162.499999999975));
#39365=CARTESIAN_POINT('',(-98.9999999999911,-100.749999999987,-162.499999999975));
#39366=CARTESIAN_POINT('Origin',(-99.1999999999909,-102.915063509438,-163.749999999975));
#39367=CARTESIAN_POINT('',(-98.9999999999908,-103.636751345888,-164.999999999975));
#39368=CARTESIAN_POINT('',(-99.1999999999908,-103.636751345888,-164.999999999975));
#39369=CARTESIAN_POINT('',(-98.999999999991,-102.193375672987,-162.499999999975));
#39370=CARTESIAN_POINT('Origin',(-99.1999999999909,-102.915063509438,-166.249999999975));
#39371=CARTESIAN_POINT('',(-98.9999999999908,-103.636751345888,-164.999999999975));
#39372=CARTESIAN_POINT('Origin',(-75.8348017621055,64.2500000000171,-140.499999999994));
#39373=CARTESIAN_POINT('',(-77.0000000000051,59.500000000017,-140.499999999993));
#39374=CARTESIAN_POINT('Origin',(-75.7841409691556,65.2500000000167,-143.999999999994));
#39375=CARTESIAN_POINT('',(-77.0000000000051,59.5000000000166,-143.999999999993));
#39376=CARTESIAN_POINT('Origin',(-75.8348017621055,64.2500000000171,-140.499999999994));
#39377=CARTESIAN_POINT('',(-77.0000000000053,59.5000000000123,-172.499999999994));
#39378=CARTESIAN_POINT('',(-74.6696035242059,69.0000000000135,-172.499999999995));
#39379=CARTESIAN_POINT('',(-77.0000000000051,59.5000000000133,-172.499999999994));
#39380=CARTESIAN_POINT('',(-77.0000000000051,59.500000000017,-140.499999999993));
#39381=CARTESIAN_POINT('',(-74.6696035242059,69.0000000000172,-140.499999999994));
#39382=CARTESIAN_POINT('Origin',(-5.91193760612896E-12,69.0000000000237,
-140.499999999994));
#39383=CARTESIAN_POINT('',(74.6696035241941,69.0000000000265,-172.499999999995));
#39384=CARTESIAN_POINT('',(-5.91193760612896E-12,69.00000000002,-172.499999999995));
#39385=CARTESIAN_POINT('',(74.6696035241941,69.0000000000302,-140.499999999994));
#39386=CARTESIAN_POINT('Origin',(75.8348017620945,64.2500000000304,-140.499999999994));
#39387=CARTESIAN_POINT('',(76.999999999995,59.5000000000266,-172.499999999994));
#39388=CARTESIAN_POINT('',(74.6696035241941,69.0000000000265,-172.499999999995));
#39389=CARTESIAN_POINT('',(76.9999999999949,59.5000000000304,-140.499999999993));
#39390=CARTESIAN_POINT('Origin',(75.7841409691445,65.2500000000299,-143.999999999994));
#39391=CARTESIAN_POINT('',(76.9999999999949,59.50000000003,-143.999999999993));
#39392=CARTESIAN_POINT('Origin',(75.8348017620945,64.2500000000304,-140.499999999994));
#39393=CARTESIAN_POINT('',(76.9999999999949,59.5000000000304,-140.499999999993));
#39394=CARTESIAN_POINT('Origin',(-66.0000000000025,29.5000000000292,-43.49999999999));
#39395=CARTESIAN_POINT('Origin',(85.0000000000052,-57.4999999999582,-47.49999999998));
#39396=CARTESIAN_POINT('',(85.0000000000047,-52.4302858857102,-77.7499999999805));
#39397=CARTESIAN_POINT('Origin',(84.4000000000047,-51.9999999999597,-60.4999999999806));
#39398=CARTESIAN_POINT('',(84.4000000000048,-53.0627460667679,-77.7499999999805));
#39399=CARTESIAN_POINT('',(84.4000000000048,-53.0627460667679,-77.7499999999805));
#39400=CARTESIAN_POINT('Origin',(-93.3999999999946,-60.9999999999807,-107.99999999998));
#39401=CARTESIAN_POINT('',(-84.9999999999938,-69.5697141142314,-107.999999999979));
#39402=CARTESIAN_POINT('',(-84.9999999999953,-52.4302858857286,-107.99999999998));
#39403=CARTESIAN_POINT('',(-84.9999999999949,-57.49999999998,-107.99999999998));
#39404=CARTESIAN_POINT('Origin',(-93.3999999999946,-60.9999999999807,-107.99999999998));
#39405=CARTESIAN_POINT('Origin',(-93.3999999999967,-36.9999999999807,-107.999999999982));
#39406=CARTESIAN_POINT('',(-84.9999999999959,-45.5697141142313,-107.999999999981));
#39407=CARTESIAN_POINT('',(-84.9999999999974,-28.4302858857285,-107.999999999983));
#39408=CARTESIAN_POINT('',(-84.9999999999949,-57.49999999998,-107.99999999998));
#39409=CARTESIAN_POINT('Origin',(-93.3999999999967,-36.9999999999807,-107.999999999982));
#39410=CARTESIAN_POINT('Origin',(-84.4,2.24700900247621E-11,-87.4999999999866));
#39411=CARTESIAN_POINT('',(-84.4,4.46250000002703,-47.4999999999871));
#39412=CARTESIAN_POINT('Origin',(-77.0000000000058,68.0000000000177,-137.259999999994));
#39413=CARTESIAN_POINT('',(-77.0000000000051,59.5000000000271,-53.2599999999935));
#39414=CARTESIAN_POINT('',(-77.0000000000051,59.5000000000277,-47.4999999999935));
#39415=CARTESIAN_POINT('',(-77.0000000000058,68.0000000000272,-53.2599999999944));
#39416=CARTESIAN_POINT('Origin',(-71.0000000000058,68.0000000000277,-53.2599999999944));
#39417=CARTESIAN_POINT('',(-72.680000000005,59.5000000000281,-47.4999999999935));
#39418=CARTESIAN_POINT('',(-71.0000000000051,59.5000000000283,-47.2599999999935));
#39419=CARTESIAN_POINT('Origin',(-71.0000000000051,59.5000000000276,-53.2599999999935));
#39420=CARTESIAN_POINT('',(-71.0000000000058,68.0000000000282,-47.2599999999944));
#39421=CARTESIAN_POINT('Origin',(-71.0000000000051,59.5000000000275,-53.2599999999935));
#39422=CARTESIAN_POINT('Origin',(74.4999999999942,68.0000000000409,-47.2599999999944));
#39423=CARTESIAN_POINT('',(70.9999999999949,59.5000000000407,-47.2599999999935));
#39424=CARTESIAN_POINT('',(70.9999999999949,59.5000000000407,-47.2599999999935));
#39425=CARTESIAN_POINT('',(-77.0000000000051,59.5000000000277,-47.2599999999935));
#39426=CARTESIAN_POINT('Origin',(70.9999999999949,59.50000000004,-53.2599999999935));
#39427=CARTESIAN_POINT('',(76.9999999999949,59.5000000000407,-53.2599999999935));
#39428=CARTESIAN_POINT('',(72.6799999999949,59.5000000000408,-47.4999999999935));
#39429=CARTESIAN_POINT('Origin',(70.9999999999949,59.50000000004,-53.2599999999935));
#39430=CARTESIAN_POINT('',(76.9999999999949,59.5000000000408,-53.2599999999935));
#39431=CARTESIAN_POINT('Origin',(70.9999999999949,59.50000000004,-53.2599999999935));
#39432=CARTESIAN_POINT('Origin',(-5.07927033766009E-12,59.5000000000344,
-47.4999999999935));
#39433=CARTESIAN_POINT('',(76.9999999999949,59.5000000000411,-47.4999999999935));
#39434=CARTESIAN_POINT('',(-77.000000000005,59.500000000028,-47.4999999999935));
#39435=CARTESIAN_POINT('Origin',(76.9999999999949,59.5000000000311,-137.259999999993));
#39436=CARTESIAN_POINT('',(76.9999999999949,59.5000000000414,-47.4999999999935));
#39437=CARTESIAN_POINT('Origin',(93.4000000000055,-60.9999999999644,-107.99999999998));
#39438=CARTESIAN_POINT('',(85.0000000000047,-52.4302858857137,-107.99999999998));
#39439=CARTESIAN_POINT('',(85.0000000000062,-69.5697141142165,-107.999999999979));
#39440=CARTESIAN_POINT('',(85.0000000000052,-57.4999999999652,-107.99999999998));
#39441=CARTESIAN_POINT('Origin',(93.4000000000055,-60.9999999999644,-107.99999999998));
#39442=CARTESIAN_POINT('Origin',(93.4000000000033,-36.9999999999644,-107.999999999982));
#39443=CARTESIAN_POINT('',(85.0000000000026,-28.4302858857138,-107.999999999983));
#39444=CARTESIAN_POINT('',(85.0000000000041,-45.5697141142166,-107.999999999981));
#39445=CARTESIAN_POINT('',(85.0000000000052,-57.4999999999652,-107.99999999998));
#39446=CARTESIAN_POINT('Origin',(93.4000000000033,-36.9999999999644,-107.999999999982));
#39447=CARTESIAN_POINT('Origin',(-26.6999999999944,-62.6999999999668,-37.4999999999794));
#39448=CARTESIAN_POINT('',(-41.0454358677504,-48.0555993716003,-37.499999999981));
#39449=CARTESIAN_POINT('Origin',(-4.16333634234434E-12,49.0000000000356,
-37.4999999999922));
#39450=CARTESIAN_POINT('Origin',(-26.6999999999944,-62.6999999999668,-37.4999999999794));
#39451=CARTESIAN_POINT('Origin',(38.0550000000051,-57.5569999999592,-21.24999999998));
#39452=CARTESIAN_POINT('',(44.6720415240432,-35.0078367900033,-6.99999999998255));
#39453=CARTESIAN_POINT('Origin',(38.0550000000051,-57.5569999999576,-6.99999999997997));
#39454=CARTESIAN_POINT('',(50.3997394425481,-37.5605651153198,-42.4999999999823));
#39455=CARTESIAN_POINT('Origin',(38.0550000000051,-57.5569999999617,-42.49999999998));
#39456=CARTESIAN_POINT('Ctrl Pts',(44.6720415240431,-35.0078367900032,-6.99999999998257));
#39457=CARTESIAN_POINT('Ctrl Pts',(45.2291351252888,-35.1713156498573,-10.284076887157));
#39458=CARTESIAN_POINT('Ctrl Pts',(45.7750777634791,-35.3550218145083,-13.5491785717897));
#39459=CARTESIAN_POINT('Ctrl Pts',(47.3525593525942,-35.9434876571267,-23.0977381265645));
#39460=CARTESIAN_POINT('Ctrl Pts',(48.5132847234971,-36.4730775652569,-30.3142603319532));
#39461=CARTESIAN_POINT('Ctrl Pts',(49.8914593873258,-37.2534035206445,-39.187988167187));
#39462=CARTESIAN_POINT('Ctrl Pts',(50.1472572750543,-37.4046960021711,-40.8480746317634));
#39463=CARTESIAN_POINT('Ctrl Pts',(50.3997394425481,-37.5605651153197,-42.4999999999823));
#39464=CARTESIAN_POINT('Origin',(1.11022302462516E-13,3.90956798185238E-11,
-6.9999999999866));
#39465=CARTESIAN_POINT('',(41.8306113344324,41.8306113344787,-6.99999999999143));
#39466=CARTESIAN_POINT('Origin',(-49.,3.4821321173717E-11,-6.9999999999866));
#39467=CARTESIAN_POINT('',(-41.8306113344394,41.8306113344714,-6.99999999999143));
#39468=CARTESIAN_POINT('Origin',(4.38538094726937E-12,-48.9999999999609,
-6.99999999998097));
#39469=CARTESIAN_POINT('',(-41.8306113344321,-41.8306113344005,-6.99999999998177));
#39470=CARTESIAN_POINT('Origin',(49.,4.33700384633307E-11,-6.9999999999866));
#39471=CARTESIAN_POINT('',(-35.8473473659403,-44.3539912741743,-6.99999999998147));
#39472=CARTESIAN_POINT('Origin',(-4.16333634234434E-12,49.0000000000391,
-6.99999999999224));
#39473=CARTESIAN_POINT('Origin',(-26.6999999999944,-62.6999999999632,-6.99999999997936));
#39474=CARTESIAN_POINT('Origin',(-26.6999999999944,-62.6999999999646,-18.7499999999794));
#39475=CARTESIAN_POINT('Ctrl Pts',(-41.0454358677504,-48.0555993716003,
-37.499999999981));
#39476=CARTESIAN_POINT('Ctrl Pts',(-40.5741646895959,-47.5939491727217,
-34.0475842300223));
#39477=CARTESIAN_POINT('Ctrl Pts',(-40.0664661275859,-47.1411670911225,
-30.5660187146972));
#39478=CARTESIAN_POINT('Ctrl Pts',(-38.6752029150759,-46.0261353656994,
-21.709527141894));
#39479=CARTESIAN_POINT('Ctrl Pts',(-37.7390814105853,-45.3849092793414,
-16.3423326679795));
#39480=CARTESIAN_POINT('Ctrl Pts',(-36.4217135929675,-44.6490164361965,
-9.73375317041888));
#39481=CARTESIAN_POINT('Ctrl Pts',(-36.1385428528838,-44.499181779111,-8.36069357089042));
#39482=CARTESIAN_POINT('Ctrl Pts',(-35.8473473659402,-44.3539912741743,
-6.99999999998149));
#39483=CARTESIAN_POINT('Origin',(38.0550000000051,-57.5569999999617,-42.49999999998));
#39484=CARTESIAN_POINT('Origin',(-49.,3.07412515582195E-11,-42.4999999999866));
#39485=CARTESIAN_POINT('Origin',(-98.9999999999911,-100.749999999988,-164.999999999975));
#39486=CARTESIAN_POINT('Origin',(1.83186799063151E-12,-19.6933104181538,
-140.499999999984));
#39487=CARTESIAN_POINT('',(-85.,1.63083522380925E-11,-140.499999999987));
#39488=CARTESIAN_POINT('',(-84.9999999999919,-90.9999999999837,-140.499999999976));
#39489=CARTESIAN_POINT('',(-84.9999999999949,-57.4999999999837,-140.49999999998));
#39490=CARTESIAN_POINT('',(-81.0000000000025,29.7500000000166,-140.49999999999));
#39491=CARTESIAN_POINT('',(-99.9999999999942,-65.168999999985,-140.499999999979));
#39492=CARTESIAN_POINT('',(-88.5,-2.83449999998398,-140.499999999986));
#39493=CARTESIAN_POINT('',(-94.9999999999913,-98.4999999999846,-140.499999999975));
#39494=CARTESIAN_POINT('',(-97.4999999999927,-81.8344999999848,-140.499999999977));
#39495=CARTESIAN_POINT('',(-90.6698729810919,-90.9999999999842,-140.499999999976));
#39496=CARTESIAN_POINT('',(-92.8349364905416,-94.7499999999844,-140.499999999976));
#39497=CARTESIAN_POINT('',(-67.4999999999919,-90.9999999999822,-140.499999999976));
#39498=CARTESIAN_POINT('Origin',(-88.5,-2.83449999998398,-140.499999999986));
#39499=CARTESIAN_POINT('',(-99.9999999999942,-65.1689999999854,-143.999999999979));
#39500=CARTESIAN_POINT('',(-77.0000000000051,59.5000000000166,-143.999999999993));
#39501=CARTESIAN_POINT('',(-99.9999999999942,-65.168999999985,-140.499999999979));
#39502=CARTESIAN_POINT('Origin',(1.74860126378462E-12,-18.7858057259544,
-143.999999999984));
#39503=CARTESIAN_POINT('',(-100.999999999994,-65.1689999999855,-143.999999999979));
#39504=CARTESIAN_POINT('',(-89.,-2.83449999998446,-143.999999999986));
#39505=CARTESIAN_POINT('',(-94.9999999999913,-98.499999999985,-143.999999999975));
#39506=CARTESIAN_POINT('',(-97.9999999999927,-81.8344999999852,-143.999999999977));
#39507=CARTESIAN_POINT('',(-97.4999999999927,-81.8344999999852,-143.999999999977));
#39508=CARTESIAN_POINT('Origin',(-89.,-2.83449999998446,-143.999999999986));
#39509=CARTESIAN_POINT('',(-100.999999999994,-65.1689999999867,-153.999999999979));
#39510=CARTESIAN_POINT('',(-100.999999999994,-65.1689999999867,-153.999999999979));
#39511=CARTESIAN_POINT('',(-100.999999999994,-65.1689999999855,-143.999999999979));
#39512=CARTESIAN_POINT('Origin',(1.74860126378462E-12,-18.7858057259555,
-153.999999999984));
#39513=CARTESIAN_POINT('',(-94.9999999999913,-98.4999999999861,-153.999999999975));
#39514=CARTESIAN_POINT('',(-97.9999999999927,-81.8344999999864,-153.999999999977));
#39515=CARTESIAN_POINT('',(-99.9999999999942,-65.1689999999866,-153.999999999979));
#39516=CARTESIAN_POINT('',(-88.5,-2.83449999998554,-153.999999999986));
#39517=CARTESIAN_POINT('',(-97.4999999999927,-81.8344999999864,-153.999999999977));
#39518=CARTESIAN_POINT('Origin',(-88.5,-2.83449999998398,-140.499999999986));
#39519=CARTESIAN_POINT('',(-99.9999999999942,-65.1689999999887,-172.499999999979));
#39520=CARTESIAN_POINT('',(-99.9999999999942,-65.1689999999887,-172.499999999979));
#39521=CARTESIAN_POINT('',(-99.9999999999942,-65.168999999985,-140.499999999979));
#39522=CARTESIAN_POINT('Origin',(1.83186799063151E-12,-19.6933104181575,
-172.499999999985));
#39523=CARTESIAN_POINT('',(40.0000000000088,-98.4999999999765,-172.499999999975));
#39524=CARTESIAN_POINT('',(44.330127018908,-90.9999999999761,-172.499999999976));
#39525=CARTESIAN_POINT('',(42.1650635094584,-94.7499999999763,-172.499999999976));
#39526=CARTESIAN_POINT('',(-39.9999999999913,-98.4999999999835,-172.499999999975));
#39527=CARTESIAN_POINT('',(8.71525074330748E-12,-98.49999999998,-172.499999999975));
#39528=CARTESIAN_POINT('',(-44.330127018892,-90.9999999999838,-172.499999999976));
#39529=CARTESIAN_POINT('',(-42.1650635094416,-94.7499999999837,-172.499999999976));
#39530=CARTESIAN_POINT('',(-90.6698729810919,-90.9999999999879,-172.499999999976));
#39531=CARTESIAN_POINT('',(-67.4999999999919,-90.9999999999859,-172.499999999976));
#39532=CARTESIAN_POINT('',(-94.9999999999913,-98.4999999999883,-172.499999999975));
#39533=CARTESIAN_POINT('',(-92.8349364905416,-94.7499999999881,-172.499999999976));
#39534=CARTESIAN_POINT('',(-97.4999999999927,-81.8344999999885,-172.499999999977));
#39535=CARTESIAN_POINT('',(100.000000000006,-65.1689999999712,-172.499999999979));
#39536=CARTESIAN_POINT('',(88.5,-2.83449999997224,-172.499999999986));
#39537=CARTESIAN_POINT('',(95.0000000000087,-98.4999999999717,-172.499999999975));
#39538=CARTESIAN_POINT('',(97.5000000000073,-81.8344999999715,-172.499999999977));
#39539=CARTESIAN_POINT('',(90.669872981108,-90.9999999999721,-172.499999999976));
#39540=CARTESIAN_POINT('',(92.8349364905584,-94.7499999999719,-172.499999999976));
#39541=CARTESIAN_POINT('',(67.5000000000081,-90.9999999999741,-172.499999999976));
#39542=CARTESIAN_POINT('Origin',(88.5,-2.83449999996856,-140.499999999986));
#39543=CARTESIAN_POINT('',(100.000000000006,-65.1689999999691,-153.999999999979));
#39544=CARTESIAN_POINT('',(100.000000000006,-65.1689999999691,-153.999999999979));
#39545=CARTESIAN_POINT('',(100.000000000006,-65.1689999999676,-140.499999999979));
#39546=CARTESIAN_POINT('Origin',(1.74860126378462E-12,-18.7858057259555,
-153.999999999984));
#39547=CARTESIAN_POINT('',(95.0000000000091,-98.4999999999673,-153.999999999975));
#39548=CARTESIAN_POINT('',(101.000000000006,-65.168999999969,-153.999999999979));
#39549=CARTESIAN_POINT('',(98.0000000000073,-81.8344999999693,-153.999999999977));
#39550=CARTESIAN_POINT('',(97.5000000000073,-81.8344999999693,-153.999999999977));
#39551=CARTESIAN_POINT('',(89.,-2.83449999997005,-153.999999999986));
#39552=CARTESIAN_POINT('Origin',(89.,-2.83449999996892,-143.999999999986));
#39553=CARTESIAN_POINT('',(101.000000000006,-65.1689999999679,-143.999999999979));
#39554=CARTESIAN_POINT('',(76.9999999999949,59.50000000003,-143.999999999993));
#39555=CARTESIAN_POINT('',(101.000000000006,-65.1689999999679,-143.999999999979));
#39556=CARTESIAN_POINT('Origin',(1.74860126378462E-12,-18.7858057259544,
-143.999999999984));
#39557=CARTESIAN_POINT('',(95.0000000000091,-98.4999999999662,-143.999999999975));
#39558=CARTESIAN_POINT('',(100.000000000006,-65.168999999968,-143.999999999979));
#39559=CARTESIAN_POINT('',(97.5000000000073,-81.8344999999682,-143.999999999977));
#39560=CARTESIAN_POINT('',(98.0000000000073,-81.8344999999681,-143.999999999977));
#39561=CARTESIAN_POINT('',(88.5,-2.83449999996897,-143.999999999986));
#39562=CARTESIAN_POINT('Origin',(88.5,-2.83449999996856,-140.499999999986));
#39563=CARTESIAN_POINT('',(100.000000000006,-65.1689999999675,-140.499999999979));
#39564=CARTESIAN_POINT('',(76.9999999999949,59.5000000000304,-140.499999999993));
#39565=CARTESIAN_POINT('',(100.000000000006,-65.1689999999676,-140.499999999979));
#39566=CARTESIAN_POINT('Origin',(1.83186799063151E-12,-19.6933104181538,
-140.499999999984));
#39567=CARTESIAN_POINT('',(95.0000000000087,-98.499999999968,-140.499999999975));
#39568=CARTESIAN_POINT('',(90.669872981108,-90.9999999999684,-140.499999999976));
#39569=CARTESIAN_POINT('',(92.8349364905584,-94.7499999999682,-140.499999999976));
#39570=CARTESIAN_POINT('',(97.5000000000073,-81.8344999999678,-140.499999999977));
#39571=CARTESIAN_POINT('',(85.,3.11298296168383E-11,-140.499999999987));
#39572=CARTESIAN_POINT('',(80.9999999999976,29.7500000000308,-140.49999999999));
#39573=CARTESIAN_POINT('',(85.000000000008,-90.9999999999689,-140.499999999976));
#39574=CARTESIAN_POINT('',(85.0000000000052,-57.4999999999689,-140.49999999998));
#39575=CARTESIAN_POINT('',(67.5000000000081,-90.9999999999704,-140.499999999976));
#39576=CARTESIAN_POINT('Origin',(85.0000000000052,-57.4999999999582,-47.49999999998));
#39577=CARTESIAN_POINT('',(85.0000000000041,-45.5697141142096,-47.4999999999814));
#39578=CARTESIAN_POINT('',(85.0000000000047,-52.4302858857068,-47.4999999999806));
#39579=CARTESIAN_POINT('',(85.0000000000027,-29.729655935319,-47.4999999999832));
#39580=CARTESIAN_POINT('',(85.0000000000047,-52.4302858857102,-77.7499999999805));
#39581=CARTESIAN_POINT('',(85.0000000000041,-45.5697141142131,-77.7499999999813));
#39582=CARTESIAN_POINT('Origin',(93.4000000000055,-60.9999999999609,-77.7499999999796));
#39583=CARTESIAN_POINT('',(85.0000000000062,-69.5697141142096,-47.4999999999786));
#39584=CARTESIAN_POINT('Origin',(93.4000000000055,-60.9999999999574,-47.4999999999796));
#39585=CARTESIAN_POINT('',(85.0000000000062,-69.5697141142096,-47.4999999999786));
#39586=CARTESIAN_POINT('',(85.0000000000047,-52.4302858857068,-47.4999999999806));
#39587=CARTESIAN_POINT('Origin',(-93.3999999999946,-60.9999999999772,-77.7499999999796));
#39588=CARTESIAN_POINT('',(-84.9999999999938,-69.5697141142244,-47.4999999999786));
#39589=CARTESIAN_POINT('',(-84.9999999999953,-52.4302858857216,-47.4999999999806));
#39590=CARTESIAN_POINT('Origin',(-93.3999999999946,-60.9999999999737,-47.4999999999796));
#39591=CARTESIAN_POINT('',(-84.9999999999953,-52.4302858857216,-47.4999999999806));
#39592=CARTESIAN_POINT('',(-84.9999999999938,-69.5697141142244,-47.4999999999786));
#39593=CARTESIAN_POINT('Origin',(-93.3999999999967,-36.9999999999772,-77.7499999999823));
#39594=CARTESIAN_POINT('',(-84.9999999999959,-45.5697141142244,-47.4999999999814));
#39595=CARTESIAN_POINT('',(-84.9999999999974,-28.4302858857216,-47.4999999999833));
#39596=CARTESIAN_POINT('Origin',(-93.3999999999967,-36.9999999999737,-47.4999999999823));
#39597=CARTESIAN_POINT('',(-84.9999999999974,-28.4302858857216,-47.4999999999833));
#39598=CARTESIAN_POINT('',(-84.9999999999959,-45.5697141142244,-47.4999999999814));
#39599=CARTESIAN_POINT('Origin',(-84.9999999999949,-57.499999999973,-47.49999999998));
#39600=CARTESIAN_POINT('',(-85.,2.73550713331128E-11,-47.4999999999866));
#39601=CARTESIAN_POINT('',(-84.9999999999973,-29.7296559353338,-47.4999999999832));
#39602=CARTESIAN_POINT('',(-85.,2.70220044257252E-11,-47.4999999999866));
#39603=CARTESIAN_POINT('',(-85.,2.70220044257252E-11,-47.4999999999866));
#39604=CARTESIAN_POINT('',(-84.9999999999919,-90.999999999973,-47.4999999999761));
#39605=CARTESIAN_POINT('',(-84.9999999999919,-90.999999999969,-12.4999999999761));
#39606=CARTESIAN_POINT('',(-84.9999999999973,-29.7296559353338,-47.4999999999832));
#39607=CARTESIAN_POINT('',(-84.9999999999973,-29.7296559353338,-47.4999999999832));
#39608=CARTESIAN_POINT('Origin',(-81.0000000000025,29.7500000000274,-47.49999999999));
#39609=CARTESIAN_POINT('',(-77.0000000000051,59.5000000000277,-47.4999999999935));
#39610=CARTESIAN_POINT('',(-85.,2.70220044257252E-11,-47.4999999999866));
#39611=CARTESIAN_POINT('',(-77.0000000000051,59.5000000000277,-47.4999999999935));
#39612=CARTESIAN_POINT('Origin',(-5.07927033766009E-12,59.5000000000344,
-47.4999999999935));
#39613=CARTESIAN_POINT('',(-5.07927033766009E-12,59.5000000000344,-47.4999999999935));
#39614=CARTESIAN_POINT('Origin',(-77.0000000000051,59.5000000000177,-137.259999999993));
#39615=CARTESIAN_POINT('',(-5.07927033766009E-12,59.5000000000344,-47.4999999999935));
#39616=CARTESIAN_POINT('Origin',(-5.07927033766009E-12,59.5000000000344,
-47.4999999999935));
#39617=CARTESIAN_POINT('',(76.9999999999949,59.5000000000411,-47.4999999999935));
#39618=CARTESIAN_POINT('',(-5.07927033766009E-12,59.5000000000344,-47.4999999999935));
#39619=CARTESIAN_POINT('',(76.9999999999949,59.5000000000411,-47.4999999999935));
#39620=CARTESIAN_POINT('Origin',(80.9999999999976,29.7500000000415,-47.49999999999));
#39621=CARTESIAN_POINT('',(85.,4.17602150776242E-11,-47.4999999999866));
#39622=CARTESIAN_POINT('',(76.9999999999949,59.5000000000411,-47.4999999999935));
#39623=CARTESIAN_POINT('',(85.,4.18434818044711E-11,-47.4999999999866));
#39624=CARTESIAN_POINT('Origin',(85.0000000000052,-57.4999999999582,-47.49999999998));
#39625=CARTESIAN_POINT('',(85.0000000000041,-45.5697141142131,-77.7499999999813));
#39626=CARTESIAN_POINT('',(85.000000000008,-90.9999999999582,-47.4999999999761));
#39627=CARTESIAN_POINT('',(85.0000000000027,-29.729655935319,-47.4999999999832));
#39628=CARTESIAN_POINT('',(85.000000000008,-90.9999999999541,-12.4999999999761));
#39629=CARTESIAN_POINT('',(85.0000000000026,-28.4302858857068,-47.4999999999833));
#39630=CARTESIAN_POINT('',(85.0000000000027,-29.729655935319,-47.4999999999832));
#39631=CARTESIAN_POINT('',(85.0000000000026,-28.4302858857103,-77.7499999999833));
#39632=CARTESIAN_POINT('Origin',(93.4000000000033,-36.9999999999609,-77.7499999999823));
#39633=CARTESIAN_POINT('Origin',(93.4000000000033,-36.9999999999574,-47.4999999999823));
#39634=CARTESIAN_POINT('Origin',(-49.,3.01583844702913E-11,-47.4999999999866));
#39635=CARTESIAN_POINT('',(47.1894200398715,47.1894200399139,-47.499999999992));
#39636=CARTESIAN_POINT('Ctrl Pts',(41.8306113344323,41.8306113344787,-6.99999999999148));
#39637=CARTESIAN_POINT('Ctrl Pts',(43.5801600662902,43.5801600663354,-20.1628904977639));
#39638=CARTESIAN_POINT('Ctrl Pts',(45.4545606962369,45.4545606962808,-34.3333927313629));
#39639=CARTESIAN_POINT('Ctrl Pts',(47.1894200398713,47.189420039914,-47.499999999992));
#39640=CARTESIAN_POINT('Origin',(-49.,3.01583844702913E-11,-47.4999999999866));
#39641=CARTESIAN_POINT('Origin',(4.38538094726937E-12,-48.9999999999656,
-47.499999999981));
#39642=CARTESIAN_POINT('',(-47.1894200398795,47.1894200399057,-47.499999999992));
#39643=CARTESIAN_POINT('Origin',(4.38538094726937E-12,-48.9999999999656,
-47.499999999981));
#39644=CARTESIAN_POINT('Ctrl Pts',(-41.8306113344396,41.8306113344712,-6.99999999999142));
#39645=CARTESIAN_POINT('Ctrl Pts',(-43.5801617860844,43.5801617861141,-20.1629034367356));
#39646=CARTESIAN_POINT('Ctrl Pts',(-45.4545647173523,45.4545647173802,-34.3334232493081));
#39647=CARTESIAN_POINT('Ctrl Pts',(-47.1894200398796,47.1894200399056,-47.499999999992));
#39648=CARTESIAN_POINT('Origin',(49.,3.8707101759905E-11,-47.4999999999866));
#39649=CARTESIAN_POINT('',(-47.1894200398712,-47.1894200398451,-47.4999999999812));
#39650=CARTESIAN_POINT('Ctrl Pts',(-41.8306113344323,-41.8306113344004,
-6.99999999998177));
#39651=CARTESIAN_POINT('Ctrl Pts',(-43.5801603135757,-43.5801603135456,
-20.1628923582288));
#39652=CARTESIAN_POINT('Ctrl Pts',(-45.4545609881339,-45.4545609881059,
-34.3333949466865));
#39653=CARTESIAN_POINT('Ctrl Pts',(-47.1894200398713,-47.1894200398451,
-47.4999999999812));
#39654=CARTESIAN_POINT('Origin',(49.,3.8707101759905E-11,-47.4999999999866));
#39655=CARTESIAN_POINT('Origin',(-4.16333634234434E-12,49.0000000000344,
-47.4999999999922));
#39656=CARTESIAN_POINT('Origin',(-4.16333634234434E-12,49.0000000000344,
-47.4999999999922));
#39657=CARTESIAN_POINT('Origin',(-67.4999999999919,-90.9999999999674,-12.4999999999761));
#39658=CARTESIAN_POINT('',(-90.6698729810919,-90.9999999999695,-12.4999999999761));
#39659=CARTESIAN_POINT('',(-44.330127018892,-90.9999999999654,-12.4999999999761));
#39660=CARTESIAN_POINT('',(-67.4999999999919,-90.9999999999674,-12.4999999999761));
#39661=CARTESIAN_POINT('',(-44.330127018892,-90.9999999999695,-47.4999999999761));
#39662=CARTESIAN_POINT('',(-44.330127018892,-90.9999999999654,-12.4999999999761));
#39663=CARTESIAN_POINT('',(8.07687250414801E-12,-90.9999999999656,-47.4999999999761));
#39664=CARTESIAN_POINT('',(-90.6698729810919,-90.9999999999695,-12.4999999999761));
#39665=CARTESIAN_POINT('Origin',(-42.1650635094416,-94.7499999999652,-12.4999999999757));
#39666=CARTESIAN_POINT('',(-39.9999999999913,-98.499999999965,-12.4999999999752));
#39667=CARTESIAN_POINT('',(-44.330127018892,-90.9999999999654,-12.4999999999761));
#39668=CARTESIAN_POINT('',(-39.9999999999913,-98.4999999999691,-47.4999999999753));
#39669=CARTESIAN_POINT('',(-39.9999999999913,-98.499999999965,-12.4999999999752));
#39670=CARTESIAN_POINT('',(-39.9999999999913,-98.4999999999691,-47.4999999999753));
#39671=CARTESIAN_POINT('Origin',(-92.8349364905416,-94.7499999999697,-12.4999999999757));
#39672=CARTESIAN_POINT('',(-94.9999999999913,-98.4999999999698,-12.4999999999752));
#39673=CARTESIAN_POINT('',(-94.9999999999913,-98.4999999999698,-12.4999999999752));
#39674=CARTESIAN_POINT('',(-94.9999999999913,-98.4999999999698,-12.4999999999752));
#39675=CARTESIAN_POINT('Origin',(-97.4999999999927,-81.8344999999848,-140.499999999977));
#39676=CARTESIAN_POINT('',(-94.9999999999913,-98.4999999999698,-12.4999999999752));
#39677=CARTESIAN_POINT('Origin',(-97.9999999999927,-81.8344999999852,-143.999999999977));
#39678=CARTESIAN_POINT('',(-94.9999999999913,-98.4999999999698,-12.4999999999752));
#39679=CARTESIAN_POINT('Origin',(-97.4999999999927,-81.8344999999848,-140.499999999977));
#39680=CARTESIAN_POINT('',(-94.9999999999913,-98.4999999999698,-12.4999999999752));
#39681=CARTESIAN_POINT('',(-94.9999999999913,-98.4999999999698,-12.4999999999752));
#39682=CARTESIAN_POINT('Origin',(-92.8349364905416,-94.7499999999697,-12.4999999999757));
#39683=CARTESIAN_POINT('',(-94.9999999999913,-98.4999999999929,-212.499999999975));
#39684=CARTESIAN_POINT('',(-90.6698729810919,-90.9999999999925,-212.499999999976));
#39685=CARTESIAN_POINT('',(-94.9999999999913,-98.4999999999929,-212.499999999975));
#39686=CARTESIAN_POINT('',(-94.9999999999913,-98.4999999999698,-12.4999999999752));
#39687=CARTESIAN_POINT('',(-90.6698729810919,-90.9999999999695,-12.4999999999761));
#39688=CARTESIAN_POINT('Origin',(-67.4999999999919,-90.9999999999674,-12.4999999999761));
#39689=CARTESIAN_POINT('',(-44.330127018892,-90.9999999999885,-212.499999999976));
#39690=CARTESIAN_POINT('',(-67.4999999999919,-90.9999999999905,-212.499999999976));
#39691=CARTESIAN_POINT('',(-44.330127018892,-90.9999999999654,-12.4999999999761));
#39692=CARTESIAN_POINT('Origin',(-42.1650635094416,-94.7499999999652,-12.4999999999757));
#39693=CARTESIAN_POINT('',(-39.9999999999913,-98.4999999999881,-212.499999999975));
#39694=CARTESIAN_POINT('',(-44.330127018892,-90.9999999999885,-212.499999999976));
#39695=CARTESIAN_POINT('',(-39.9999999999913,-98.499999999965,-12.4999999999752));
#39696=CARTESIAN_POINT('Origin',(8.71525074330748E-12,-98.4999999999763,
-140.499999999975));
#39697=CARTESIAN_POINT('',(40.0000000000088,-98.4999999999728,-140.499999999975));
#39698=CARTESIAN_POINT('',(40.0000000000088,-98.4999999999581,-12.4999999999752));
#39699=CARTESIAN_POINT('',(-39.9999999999913,-98.4999999999798,-140.499999999975));
#39700=CARTESIAN_POINT('',(8.71525074330748E-12,-98.4999999999763,-140.499999999975));
#39701=CARTESIAN_POINT('',(-39.9999999999913,-98.499999999965,-12.4999999999752));
#39702=CARTESIAN_POINT('Origin',(42.1650635094584,-94.7499999999579,-12.4999999999757));
#39703=CARTESIAN_POINT('',(40.0000000000088,-98.4999999999811,-212.499999999975));
#39704=CARTESIAN_POINT('',(44.330127018908,-90.9999999999807,-212.499999999976));
#39705=CARTESIAN_POINT('',(40.0000000000088,-98.4999999999811,-212.499999999975));
#39706=CARTESIAN_POINT('',(40.0000000000088,-98.4999999999581,-12.4999999999752));
#39707=CARTESIAN_POINT('',(44.330127018908,-90.9999999999577,-12.4999999999761));
#39708=CARTESIAN_POINT('Origin',(67.5000000000081,-90.9999999999557,-12.4999999999761));
#39709=CARTESIAN_POINT('',(90.669872981108,-90.9999999999767,-212.499999999976));
#39710=CARTESIAN_POINT('',(67.5000000000081,-90.9999999999787,-212.499999999976));
#39711=CARTESIAN_POINT('',(90.669872981108,-90.9999999999536,-12.4999999999761));
#39712=CARTESIAN_POINT('Origin',(92.8349364905584,-94.7499999999534,-12.4999999999757));
#39713=CARTESIAN_POINT('',(95.0000000000087,-98.4999999999763,-212.499999999975));
#39714=CARTESIAN_POINT('',(90.669872981108,-90.9999999999767,-212.499999999976));
#39715=CARTESIAN_POINT('',(95.0000000000087,-98.4999999999533,-12.4999999999752));
#39716=CARTESIAN_POINT('Origin',(97.5000000000073,-81.8344999999678,-140.499999999977));
#39717=CARTESIAN_POINT('',(95.0000000000087,-98.4999999999533,-12.4999999999752));
#39718=CARTESIAN_POINT('Origin',(98.0000000000073,-81.8344999999681,-143.999999999977));
#39719=CARTESIAN_POINT('',(95.0000000000087,-98.4999999999533,-12.4999999999752));
#39720=CARTESIAN_POINT('Origin',(97.5000000000073,-81.8344999999678,-140.499999999977));
#39721=CARTESIAN_POINT('',(95.0000000000087,-98.4999999999533,-12.4999999999752));
#39722=CARTESIAN_POINT('Origin',(67.5000000000081,-90.9999999999557,-12.4999999999761));
#39723=CARTESIAN_POINT('',(44.330127018908,-90.9999999999577,-12.4999999999761));
#39724=CARTESIAN_POINT('',(90.669872981108,-90.9999999999536,-12.4999999999761));
#39725=CARTESIAN_POINT('',(67.5000000000081,-90.9999999999557,-12.4999999999761));
#39726=CARTESIAN_POINT('',(90.669872981108,-90.9999999999536,-12.4999999999761));
#39727=CARTESIAN_POINT('',(44.330127018908,-90.9999999999617,-47.4999999999761));
#39728=CARTESIAN_POINT('',(8.07687250414801E-12,-90.9999999999656,-47.4999999999761));
#39729=CARTESIAN_POINT('',(44.330127018908,-90.9999999999577,-12.4999999999761));
#39730=CARTESIAN_POINT('Origin',(92.8349364905584,-94.7499999999534,-12.4999999999757));
#39731=CARTESIAN_POINT('',(95.0000000000087,-98.4999999999533,-12.4999999999752));
#39732=CARTESIAN_POINT('',(90.669872981108,-90.9999999999536,-12.4999999999761));
#39733=CARTESIAN_POINT('',(95.0000000000087,-98.4999999999533,-12.4999999999752));
#39734=CARTESIAN_POINT('Origin',(42.1650635094584,-94.7499999999579,-12.4999999999757));
#39735=CARTESIAN_POINT('',(40.0000000000088,-98.4999999999581,-12.4999999999752));
#39736=CARTESIAN_POINT('',(40.0000000000088,-98.4999999999581,-12.4999999999752));
#39737=CARTESIAN_POINT('',(40.0000000000088,-98.4999999999621,-47.4999999999753));
#39738=CARTESIAN_POINT('',(44.330127018908,-90.9999999999617,-47.4999999999761));
#39739=CARTESIAN_POINT('',(40.0000000000088,-98.4999999999581,-12.4999999999752));
#39740=CARTESIAN_POINT('Origin',(2.72004641033164E-12,-29.7296559353265,
-47.4999999999832));
#39741=CARTESIAN_POINT('',(-39.9999999999898,-114.999999999969,-47.4999999999733));
#39742=CARTESIAN_POINT('',(-39.9999999999905,-106.749999999969,-47.4999999999743));
#39743=CARTESIAN_POINT('',(40.0000000000102,-114.999999999962,-47.4999999999733));
#39744=CARTESIAN_POINT('',(1.01585406753202E-11,-114.999999999966,-47.4999999999733));
#39745=CARTESIAN_POINT('',(40.0000000000095,-106.749999999962,-47.4999999999743));
#39746=CARTESIAN_POINT('Origin',(-39.9999999999905,-106.749999999965,-12.4999999999743));
#39747=CARTESIAN_POINT('',(-39.9999999999898,-114.999999999965,-12.4999999999733));
#39748=CARTESIAN_POINT('',(-39.9999999999908,-103.559005108899,-12.4999999999747));
#39749=CARTESIAN_POINT('',(-39.9999999999898,-114.999999999969,-47.4999999999733));
#39750=CARTESIAN_POINT('Origin',(-67.4999999999909,-103.559005108901,-12.4999999999747));
#39751=CARTESIAN_POINT('',(-94.9999999999898,-114.99999999997,-12.4999999999733));
#39752=CARTESIAN_POINT('',(-94.9999999999906,-106.74999999997,-12.4999999999743));
#39753=CARTESIAN_POINT('',(1.01585406753202E-11,-114.999999999962,-12.4999999999733));
#39754=CARTESIAN_POINT('Origin',(-94.9999999999906,-106.74999999997,-12.4999999999743));
#39755=CARTESIAN_POINT('',(-94.9999999999898,-114.999999999993,-212.499999999974));
#39756=CARTESIAN_POINT('',(-94.9999999999908,-103.559005108927,-212.499999999974));
#39757=CARTESIAN_POINT('',(-94.9999999999898,-114.999999999974,-47.4999999999733));
#39758=CARTESIAN_POINT('Origin',(-67.4999999999909,-103.559005108924,-212.499999999974));
#39759=CARTESIAN_POINT('',(-39.9999999999898,-114.999999999988,-212.499999999974));
#39760=CARTESIAN_POINT('',(-39.9999999999905,-106.749999999988,-212.499999999974));
#39761=CARTESIAN_POINT('',(1.01585406753202E-11,-114.999999999985,-212.499999999974));
#39762=CARTESIAN_POINT('Origin',(-39.9999999999905,-106.749999999965,-12.4999999999743));
#39763=CARTESIAN_POINT('',(-39.9999999999898,-114.99999999998,-140.499999999973));
#39764=CARTESIAN_POINT('',(-39.9999999999973,-29.7296559353406,-140.499999999983));
#39765=CARTESIAN_POINT('',(-39.9999999999898,-114.999999999969,-47.4999999999733));
#39766=CARTESIAN_POINT('Origin',(2.72004641033164E-12,-29.7296559353372,
-140.499999999983));
#39767=CARTESIAN_POINT('',(40.0000000000102,-114.999999999973,-140.499999999973));
#39768=CARTESIAN_POINT('',(40.0000000000095,-106.749999999973,-140.499999999974));
#39769=CARTESIAN_POINT('',(1.01585406753202E-11,-114.999999999976,-140.499999999973));
#39770=CARTESIAN_POINT('Origin',(40.0000000000095,-106.749999999958,-12.4999999999743));
#39771=CARTESIAN_POINT('',(40.0000000000102,-114.999999999981,-212.499999999974));
#39772=CARTESIAN_POINT('',(40.0000000000092,-103.559005108915,-212.499999999974));
#39773=CARTESIAN_POINT('',(40.0000000000102,-114.999999999962,-47.4999999999733));
#39774=CARTESIAN_POINT('Origin',(67.5000000000092,-103.559005108913,-212.499999999974));
#39775=CARTESIAN_POINT('',(95.0000000000102,-114.999999999976,-212.499999999974));
#39776=CARTESIAN_POINT('',(95.0000000000094,-106.749999999976,-212.499999999974));
#39777=CARTESIAN_POINT('',(1.01585406753202E-11,-114.999999999985,-212.499999999974));
#39778=CARTESIAN_POINT('Origin',(95.0000000000094,-106.749999999953,-12.4999999999743));
#39779=CARTESIAN_POINT('',(95.0000000000102,-114.999999999953,-12.4999999999733));
#39780=CARTESIAN_POINT('',(95.0000000000092,-103.559005108887,-12.4999999999747));
#39781=CARTESIAN_POINT('',(95.0000000000102,-114.999999999957,-47.4999999999733));
#39782=CARTESIAN_POINT('Origin',(67.5000000000092,-103.55900510889,-12.4999999999747));
#39783=CARTESIAN_POINT('',(40.0000000000102,-114.999999999958,-12.4999999999733));
#39784=CARTESIAN_POINT('',(40.0000000000095,-106.749999999958,-12.4999999999743));
#39785=CARTESIAN_POINT('',(1.01585406753202E-11,-114.999999999962,-12.4999999999733));
#39786=CARTESIAN_POINT('Origin',(40.0000000000095,-106.749999999958,-12.4999999999743));
#39787=CARTESIAN_POINT('',(40.0000000000102,-114.999999999962,-47.4999999999733));
#39788=CARTESIAN_POINT('Origin',(1.01585406753202E-11,-114.999999999966,
-47.4999999999733));
#39789=CARTESIAN_POINT('',(0.,0.,0.));
#39790=CARTESIAN_POINT('Origin',(3.,0.,0.));
#39791=CARTESIAN_POINT('',(3.,2.44929359829471E-16,-2.));
#39792=CARTESIAN_POINT('',(3.,-2.44929359829471E-16,2.));
#39793=CARTESIAN_POINT('Origin',(3.,0.,0.));
#39794=CARTESIAN_POINT('Origin',(3.,0.,0.));
#39795=CARTESIAN_POINT('',(2.8,-2.69422295812418E-16,2.2));
#39796=CARTESIAN_POINT('Origin',(3.,-2.69422295812418E-16,2.2));
#39797=CARTESIAN_POINT('Origin',(2.8,0.,0.));
#39798=CARTESIAN_POINT('Origin',(0.,0.,0.));
#39799=CARTESIAN_POINT('',(2.4,-3.03108891324553,1.75000000000001));
#39800=CARTESIAN_POINT('',(2.4,0.,3.5));
#39801=CARTESIAN_POINT('Origin',(2.4,0.,0.));
#39802=CARTESIAN_POINT('',(2.4,-3.03108891324553,-1.75));
#39803=CARTESIAN_POINT('Origin',(2.4,0.,0.));
#39804=CARTESIAN_POINT('',(2.4,3.7557864968429E-16,-3.5));
#39805=CARTESIAN_POINT('Origin',(2.4,0.,0.));
#39806=CARTESIAN_POINT('',(2.8,-4.28626379701574E-16,-3.5));
#39807=CARTESIAN_POINT('',(0.,-4.28626379701574E-16,-3.5));
#39808=CARTESIAN_POINT('Origin',(2.8,0.,0.));
#39809=CARTESIAN_POINT('',(2.4,3.03108891324553,-1.75));
#39810=CARTESIAN_POINT('Origin',(2.4,0.,0.));
#39811=CARTESIAN_POINT('',(2.4,3.03108891324553,1.75));
#39812=CARTESIAN_POINT('Origin',(2.4,0.,0.));
#39813=CARTESIAN_POINT('Origin',(2.4,0.,0.));
#39814=CARTESIAN_POINT('Origin',(27.8,0.,0.));
#39815=CARTESIAN_POINT('',(27.41,-2.44929359829471E-16,-2.));
#39816=CARTESIAN_POINT('Origin',(27.41,0.,0.));
#39817=CARTESIAN_POINT('',(27.8,-1.97168134662724E-16,-1.61));
#39818=CARTESIAN_POINT('',(27.8,-1.97168134662724E-16,-1.61));
#39819=CARTESIAN_POINT('Origin',(27.8,0.,0.));
#39820=CARTESIAN_POINT('Origin',(0.,0.,0.));
#39821=CARTESIAN_POINT('',(0.,-2.44929359829471E-16,-2.));
#39822=CARTESIAN_POINT('Origin',(2.8,4.04145188432738,0.));
#39823=CARTESIAN_POINT('Origin',(27.8,0.,0.));
#39824=CARTESIAN_POINT('Origin',(2.4,3.5,0.));
#39825=CARTESIAN_POINT('',(2.4,2.02072594216369,-3.5));
#39826=CARTESIAN_POINT('',(2.4,2.02072594216369,-3.5));
#39827=CARTESIAN_POINT('',(2.4,2.02072594216369,-3.5));
#39828=CARTESIAN_POINT('Origin',(2.4,3.5,0.));
#39829=CARTESIAN_POINT('',(2.4,4.04145188432738,0.));
#39830=CARTESIAN_POINT('',(2.4,2.02072594216369,-3.5));
#39831=CARTESIAN_POINT('',(2.4,4.04145188432738,0.));
#39832=CARTESIAN_POINT('Origin',(2.4,3.5,0.));
#39833=CARTESIAN_POINT('',(2.4,2.02072594216369,3.5));
#39834=CARTESIAN_POINT('',(2.4,4.04145188432738,0.));
#39835=CARTESIAN_POINT('',(2.4,2.02072594216369,3.5));
#39836=CARTESIAN_POINT('Origin',(2.4,3.5,0.));
#39837=CARTESIAN_POINT('',(2.4,-2.02072594216369,3.5));
#39838=CARTESIAN_POINT('',(2.4,2.02072594216369,3.5));
#39839=CARTESIAN_POINT('',(2.4,-4.04145188432739,0.));
#39840=CARTESIAN_POINT('Origin',(2.4,3.5,0.));
#39841=CARTESIAN_POINT('',(2.4,-4.04145188432739,0.));
#39842=CARTESIAN_POINT('',(2.4,-4.04145188432739,0.));
#39843=CARTESIAN_POINT('',(2.4,-2.0207259421637,-3.5));
#39844=CARTESIAN_POINT('Origin',(2.4,3.5,0.));
#39845=CARTESIAN_POINT('',(2.4,-2.0207259421637,-3.5));
#39846=CARTESIAN_POINT('',(2.4,-2.0207259421637,-3.5));
#39847=CARTESIAN_POINT('',(2.4,2.02072594216369,-3.5));
#39848=CARTESIAN_POINT('Origin',(0.,4.04145188432738,0.));
#39849=CARTESIAN_POINT('',(0.,3.7557864968429E-16,-3.5));
#39850=CARTESIAN_POINT('',(0.,3.03108891324553,-1.75));
#39851=CARTESIAN_POINT('Origin',(0.,0.,0.));
#39852=CARTESIAN_POINT('',(0.,-3.03108891324553,-1.75));
#39853=CARTESIAN_POINT('Origin',(0.,0.,0.));
#39854=CARTESIAN_POINT('',(0.,-3.03108891324553,1.75000000000001));
#39855=CARTESIAN_POINT('Origin',(0.,0.,0.));
#39856=CARTESIAN_POINT('',(0.,0.,3.5));
#39857=CARTESIAN_POINT('Origin',(0.,0.,0.));
#39858=CARTESIAN_POINT('',(0.,3.03108891324553,1.75));
#39859=CARTESIAN_POINT('Origin',(0.,0.,0.));
#39860=CARTESIAN_POINT('Origin',(0.,0.,0.));
#39861=CARTESIAN_POINT('Origin',(0.,0.,0.));
#39862=CARTESIAN_POINT('',(0.312607391169643,4.04145188432738,-2.66911020840508E-16));
#39863=CARTESIAN_POINT('Ctrl Pts',(-4.82369624061666E-16,3.03108891324553,
1.75));
#39864=CARTESIAN_POINT('Ctrl Pts',(-2.22044604925031E-16,3.5000000000009,
0.937822173507365));
#39865=CARTESIAN_POINT('Ctrl Pts',(0.312607391170941,4.04145188432963,-3.89552910831185E-12));
#39866=CARTESIAN_POINT('Ctrl Pts',(0.312607391170943,4.04145188432964,3.89877711483892E-12));
#39867=CARTESIAN_POINT('Ctrl Pts',(3.62259049097696E-16,3.5000000000009,
-0.937822173507367));
#39868=CARTESIAN_POINT('Ctrl Pts',(9.64739248123335E-16,3.03108891324553,
-1.75000000000001));
#39869=CARTESIAN_POINT('Origin',(0.,0.,0.));
#39870=CARTESIAN_POINT('',(0.31260739116964,2.02072594216368,3.5));
#39871=CARTESIAN_POINT('Ctrl Pts',(4.82369624061667E-16,-3.85895699249333E-15,
3.5));
#39872=CARTESIAN_POINT('Ctrl Pts',(-2.77555756156289E-17,0.937822173510732,
3.5));
#39873=CARTESIAN_POINT('Ctrl Pts',(0.312607391170938,2.02072594216818,3.5));
#39874=CARTESIAN_POINT('Ctrl Pts',(0.312607391170937,2.02072594216144,3.50000000000389));
#39875=CARTESIAN_POINT('Ctrl Pts',(-8.6328561492913E-16,2.56217782649016,
2.56217782649263));
#39876=CARTESIAN_POINT('Ctrl Pts',(-4.82369624061666E-16,3.03108891324553,
1.75));
#39877=CARTESIAN_POINT('Origin',(0.,0.,0.));
#39878=CARTESIAN_POINT('',(0.312607391169641,-2.02072594216369,3.5));
#39879=CARTESIAN_POINT('Ctrl Pts',(0.312607391170939,-2.02072594216818,
3.5));
#39880=CARTESIAN_POINT('Ctrl Pts',(1.03932589631759E-15,-0.937822173510737,
3.5));
#39881=CARTESIAN_POINT('Ctrl Pts',(4.82369624061667E-16,-3.85895699249333E-15,
3.5));
#39882=CARTESIAN_POINT('Ctrl Pts',(1.74858988722354E-15,-3.03108891324553,
1.75000000000001));
#39883=CARTESIAN_POINT('Ctrl Pts',(2.55351295663786E-15,-2.56217782649016,
2.56217782649264));
#39884=CARTESIAN_POINT('Ctrl Pts',(0.312607391170939,-2.02072594216144,
3.5000000000039));
#39885=CARTESIAN_POINT('Origin',(0.,0.,0.));
#39886=CARTESIAN_POINT('',(0.312607391169646,-4.04145188432739,1.06150963257362E-16));
#39887=CARTESIAN_POINT('Ctrl Pts',(0.312607391170944,-4.04145188432964,
-3.89461966648427E-12));
#39888=CARTESIAN_POINT('Ctrl Pts',(1.05543578901031E-15,-3.5000000000009,
0.937822173507371));
#39889=CARTESIAN_POINT('Ctrl Pts',(1.74858988722354E-15,-3.03108891324553,
1.75000000000001));
#39890=CARTESIAN_POINT('Ctrl Pts',(2.83392154136229E-15,-3.03108891324554,
-1.75000000000001));
#39891=CARTESIAN_POINT('Ctrl Pts',(1.97064586870965E-15,-3.50000000000091,
-0.937822173507369));
#39892=CARTESIAN_POINT('Ctrl Pts',(0.312607391170943,-4.04145188432964,
3.89397006517885E-12));
#39893=CARTESIAN_POINT('Origin',(0.,0.,0.));
#39894=CARTESIAN_POINT('',(0.31260739116964,2.02072594216369,-3.5));
#39895=CARTESIAN_POINT('Ctrl Pts',(9.64739248123335E-16,3.03108891324553,
-1.75000000000001));
#39896=CARTESIAN_POINT('Ctrl Pts',(1.52655665885959E-15,2.56217782649016,
-2.56217782649264));
#39897=CARTESIAN_POINT('Ctrl Pts',(0.312607391170938,2.02072594216144,-3.50000000000389));
#39898=CARTESIAN_POINT('Ctrl Pts',(0.312607391170937,2.02072594216818,-3.5));
#39899=CARTESIAN_POINT('Ctrl Pts',(4.11322098714103E-16,0.937822173510735,
-3.5));
#39900=CARTESIAN_POINT('Ctrl Pts',(-1.20592406015415E-16,3.85895699249333E-15,
-3.5));
#39901=CARTESIAN_POINT('Origin',(0.,0.,0.));
#39902=CARTESIAN_POINT('',(0.312607391169536,-2.02072594216386,-3.5));
#39903=CARTESIAN_POINT('Ctrl Pts',(0.312607391170909,-2.0207259421615,-3.5000000000038));
#39904=CARTESIAN_POINT('Ctrl Pts',(3.55895681952653E-15,-2.56217782649019,
-2.5621778264926));
#39905=CARTESIAN_POINT('Ctrl Pts',(2.83392154136229E-15,-3.03108891324554,
-1.75000000000001));
#39906=CARTESIAN_POINT('Ctrl Pts',(-1.20592406015415E-16,3.85895699249333E-15,
-3.5));
#39907=CARTESIAN_POINT('Ctrl Pts',(-5.82867087928207E-16,-0.937822173510786,
-3.5));
#39908=CARTESIAN_POINT('Ctrl Pts',(0.312607391170976,-2.02072594216831,
-3.5));
#39909=CARTESIAN_POINT('Origin',(2.8,2.02072594216369,-3.5));
#39910=CARTESIAN_POINT('',(2.8,-2.0207259421637,-3.5));
#39911=CARTESIAN_POINT('',(2.8,2.02072594216369,-3.5));
#39912=CARTESIAN_POINT('Origin',(2.8,-2.0207259421637,-3.5));
#39913=CARTESIAN_POINT('',(2.8,-4.04145188432739,0.));
#39914=CARTESIAN_POINT('Origin',(2.8,-4.04145188432739,0.));
#39915=CARTESIAN_POINT('',(2.8,-2.02072594216369,3.5));
#39916=CARTESIAN_POINT('Origin',(2.8,2.02072594216369,3.5));
#39917=CARTESIAN_POINT('',(2.8,2.02072594216369,3.5));
#39918=CARTESIAN_POINT('Origin',(2.8,4.04145188432738,0.));
#39919=CARTESIAN_POINT('',(2.8,4.04145188432738,0.));
#39920=CARTESIAN_POINT('Origin',(2.8,2.02072594216369,-3.5));
#39921=CARTESIAN_POINT('',(0.,0.,0.));
#39922=CARTESIAN_POINT('',(0.,0.,0.));
#39923=CARTESIAN_POINT('',(0.,0.,0.));
#39924=CARTESIAN_POINT('',(0.,0.,0.));
#39925=CARTESIAN_POINT('',(0.,0.,0.));
#39926=CARTESIAN_POINT('',(1.92093057589514,-4.57411886145564E-11,-52.5000000000137));
#39927=CARTESIAN_POINT('',(0.,267.,62.8));
#39928=CARTESIAN_POINT('',(-108.598683701239,243.916637190574,62.8));
#39929=CARTESIAN_POINT('',(-198.419668402465,178.657871897815,62.8));
#39930=CARTESIAN_POINT('',(-253.932089850806,82.5075374981103,62.8));
#39931=CARTESIAN_POINT('',(-265.537346063329,-27.9090996924645,62.8));
#39932=CARTESIAN_POINT('',(-231.228782810445,-133.500000000001,62.8));
#39933=CARTESIAN_POINT('',(-156.938662362089,-216.007537498112,62.8));
#39934=CARTESIAN_POINT('',(-55.5124214483401,-261.165409395926,62.8));
#39935=CARTESIAN_POINT('',(55.5124214483437,-261.165409395926,62.8));
#39936=CARTESIAN_POINT('',(156.938662362092,-216.00753749811,62.8));
#39937=CARTESIAN_POINT('',(231.228782810446,-133.499999999998,62.8));
#39938=CARTESIAN_POINT('',(265.537346063329,-27.9090996924609,62.8));
#39939=CARTESIAN_POINT('',(253.932089850805,82.5075374981136,62.8));
#39940=CARTESIAN_POINT('',(198.419668402462,178.657871897818,62.8));
#39941=CARTESIAN_POINT('',(108.598683701236,243.916637190576,62.8));
#39942=UNCERTAINTY_MEASURE_WITH_UNIT(LENGTH_MEASURE(0.01),#39960,
'DISTANCE_ACCURACY_VALUE',
'Maximum model space distance between geometric entities at asserted c
onnectivities');
#39943=UNCERTAINTY_MEASURE_WITH_UNIT(LENGTH_MEASURE(0.01),#39960,
'DISTANCE_ACCURACY_VALUE',
'Maximum model space distance between geometric entities at asserted c
onnectivities');
#39944=UNCERTAINTY_MEASURE_WITH_UNIT(LENGTH_MEASURE(0.01),#39960,
'DISTANCE_ACCURACY_VALUE',
'Maximum model space distance between geometric entities at asserted c
onnectivities');
#39945=UNCERTAINTY_MEASURE_WITH_UNIT(LENGTH_MEASURE(0.01),#39960,
'DISTANCE_ACCURACY_VALUE',
'Maximum model space distance between geometric entities at asserted c
onnectivities');
#39946=UNCERTAINTY_MEASURE_WITH_UNIT(LENGTH_MEASURE(0.01),#39960,
'DISTANCE_ACCURACY_VALUE',
'Maximum model space distance between geometric entities at asserted c
onnectivities');
#39947=UNCERTAINTY_MEASURE_WITH_UNIT(LENGTH_MEASURE(0.01),#39960,
'DISTANCE_ACCURACY_VALUE',
'Maximum model space distance between geometric entities at asserted c
onnectivities');
#39948=UNCERTAINTY_MEASURE_WITH_UNIT(LENGTH_MEASURE(0.01),#39960,
'DISTANCE_ACCURACY_VALUE',
'Maximum model space distance between geometric entities at asserted c
onnectivities');
#39949=UNCERTAINTY_MEASURE_WITH_UNIT(LENGTH_MEASURE(0.01),#39960,
'DISTANCE_ACCURACY_VALUE',
'Maximum model space distance between geometric entities at asserted c
onnectivities');
#39950=UNCERTAINTY_MEASURE_WITH_UNIT(LENGTH_MEASURE(0.01),#39960,
'DISTANCE_ACCURACY_VALUE',
'Maximum model space distance between geometric entities at asserted c
onnectivities');
#39951=(
GEOMETRIC_REPRESENTATION_CONTEXT(3)
GLOBAL_UNCERTAINTY_ASSIGNED_CONTEXT((#39942))
GLOBAL_UNIT_ASSIGNED_CONTEXT((#39960,#39962,#39963))
REPRESENTATION_CONTEXT('','3D')
);
#39952=(
GEOMETRIC_REPRESENTATION_CONTEXT(3)
GLOBAL_UNCERTAINTY_ASSIGNED_CONTEXT((#39943))
GLOBAL_UNIT_ASSIGNED_CONTEXT((#39960,#39962,#39963))
REPRESENTATION_CONTEXT('','3D')
);
#39953=(
GEOMETRIC_REPRESENTATION_CONTEXT(3)
GLOBAL_UNCERTAINTY_ASSIGNED_CONTEXT((#39944))
GLOBAL_UNIT_ASSIGNED_CONTEXT((#39960,#39962,#39963))
REPRESENTATION_CONTEXT('','3D')
);
#39954=(
GEOMETRIC_REPRESENTATION_CONTEXT(3)
GLOBAL_UNCERTAINTY_ASSIGNED_CONTEXT((#39945))
GLOBAL_UNIT_ASSIGNED_CONTEXT((#39960,#39962,#39963))
REPRESENTATION_CONTEXT('','3D')
);
#39955=(
GEOMETRIC_REPRESENTATION_CONTEXT(3)
GLOBAL_UNCERTAINTY_ASSIGNED_CONTEXT((#39946))
GLOBAL_UNIT_ASSIGNED_CONTEXT((#39960,#39962,#39963))
REPRESENTATION_CONTEXT('','3D')
);
#39956=(
GEOMETRIC_REPRESENTATION_CONTEXT(3)
GLOBAL_UNCERTAINTY_ASSIGNED_CONTEXT((#39947))
GLOBAL_UNIT_ASSIGNED_CONTEXT((#39960,#39962,#39963))
REPRESENTATION_CONTEXT('','3D')
);
#39957=(
GEOMETRIC_REPRESENTATION_CONTEXT(3)
GLOBAL_UNCERTAINTY_ASSIGNED_CONTEXT((#39948))
GLOBAL_UNIT_ASSIGNED_CONTEXT((#39960,#39962,#39963))
REPRESENTATION_CONTEXT('','3D')
);
#39958=(
GEOMETRIC_REPRESENTATION_CONTEXT(3)
GLOBAL_UNCERTAINTY_ASSIGNED_CONTEXT((#39949))
GLOBAL_UNIT_ASSIGNED_CONTEXT((#39960,#39962,#39963))
REPRESENTATION_CONTEXT('','3D')
);
#39959=(
GEOMETRIC_REPRESENTATION_CONTEXT(3)
GLOBAL_UNCERTAINTY_ASSIGNED_CONTEXT((#39950))
GLOBAL_UNIT_ASSIGNED_CONTEXT((#39960,#39962,#39963))
REPRESENTATION_CONTEXT('','3D')
);
#39960=(
LENGTH_UNIT()
NAMED_UNIT(*)
SI_UNIT(.MILLI.,.METRE.)
);
#39961=(
LENGTH_UNIT()
NAMED_UNIT(*)
SI_UNIT($,.METRE.)
);
#39962=(
NAMED_UNIT(*)
PLANE_ANGLE_UNIT()
SI_UNIT($,.RADIAN.)
);
#39963=(
NAMED_UNIT(*)
SI_UNIT($,.STERADIAN.)
SOLID_ANGLE_UNIT()
);
#39964=SHAPE_DEFINITION_REPRESENTATION(#39972,#40001);
#39965=SHAPE_DEFINITION_REPRESENTATION(#39973,#40002);
#39966=SHAPE_DEFINITION_REPRESENTATION(#39974,#40003);
#39967=SHAPE_DEFINITION_REPRESENTATION(#39975,#40004);
#39968=SHAPE_DEFINITION_REPRESENTATION(#39976,#40005);
#39969=SHAPE_DEFINITION_REPRESENTATION(#39977,#40006);
#39970=SHAPE_DEFINITION_REPRESENTATION(#39978,#40007);
#39971=SHAPE_DEFINITION_REPRESENTATION(#39979,#40008);
#39972=PRODUCT_DEFINITION_SHAPE('',$,#40010);
#39973=PRODUCT_DEFINITION_SHAPE('',$,#40011);
#39974=PRODUCT_DEFINITION_SHAPE('',$,#40012);
#39975=PRODUCT_DEFINITION_SHAPE('',$,#40013);
#39976=PRODUCT_DEFINITION_SHAPE('',$,#40014);
#39977=PRODUCT_DEFINITION_SHAPE('',$,#40015);
#39978=PRODUCT_DEFINITION_SHAPE('',$,#40016);
#39979=PRODUCT_DEFINITION_SHAPE('',$,#40017);
#39980=PRODUCT_DEFINITION_SHAPE($,$,#74);
#39981=PRODUCT_DEFINITION_SHAPE($,$,#75);
#39982=PRODUCT_DEFINITION_SHAPE($,$,#76);
#39983=PRODUCT_DEFINITION_SHAPE($,$,#77);
#39984=PRODUCT_DEFINITION_SHAPE($,$,#78);
#39985=PRODUCT_DEFINITION_SHAPE($,$,#79);
#39986=PRODUCT_DEFINITION_SHAPE($,$,#80);
#39987=PRODUCT_DEFINITION_SHAPE($,$,#81);
#39988=PRODUCT_DEFINITION_SHAPE($,$,#82);
#39989=PRODUCT_DEFINITION_SHAPE($,$,#83);
#39990=PRODUCT_DEFINITION_SHAPE($,$,#84);
#39991=PRODUCT_DEFINITION_SHAPE($,$,#85);
#39992=PRODUCT_DEFINITION_SHAPE($,$,#86);
#39993=PRODUCT_DEFINITION_SHAPE($,$,#87);
#39994=PRODUCT_DEFINITION_SHAPE($,$,#88);
#39995=PRODUCT_DEFINITION_SHAPE($,$,#89);
#39996=PRODUCT_DEFINITION_SHAPE($,$,#90);
#39997=PRODUCT_DEFINITION_SHAPE($,$,#91);
#39998=PRODUCT_DEFINITION_SHAPE($,$,#92);
#39999=PRODUCT_DEFINITION_SHAPE($,$,#93);
#40000=PRODUCT_DEFINITION_SHAPE($,$,#94);
#40001=SHAPE_REPRESENTATION('',(#18349,#19989,#19990,#19991,#19992,#19993,
#19994,#19995,#19996,#19997,#19998,#19999,#20000,#20001,#20002,#20003,#20004,
#20005,#20006,#20007,#20008,#20009),#39951);
#40002=SHAPE_REPRESENTATION('',(#18350),#39952);
#40003=SHAPE_REPRESENTATION('',(#18536),#39953);
#40004=SHAPE_REPRESENTATION('',(#18721),#39954);
#40005=SHAPE_REPRESENTATION('',(#18752),#39955);
#40006=SHAPE_REPRESENTATION('',(#18793),#39956);
#40007=SHAPE_REPRESENTATION('',(#18852),#39957);
#40008=SHAPE_REPRESENTATION('',(#19944),#39958);
#40009=PRODUCT_DEFINITION_CONTEXT('part definition',#40035,'design');
#40010=PRODUCT_DEFINITION('Flexible Tube Hose Pump',
'MAS-330',#40018,#40009);
#40011=PRODUCT_DEFINITION('Main Cover','Main Cover',#40019,#40009);
#40012=PRODUCT_DEFINITION('Central Rotor Drive Shaft',
'Central Rotor Drive Shaft',#40020,#40009);
#40013=PRODUCT_DEFINITION('Flexible Tubing','Flexible Tubing',#40021,#40009);
#40014=PRODUCT_DEFINITION('Motor Base','Motor Base',#40022,#40009);
#40015=PRODUCT_DEFINITION('Cover with Sight Glass',
'Cover with Sight Glass',#40023,#40009);
#40016=PRODUCT_DEFINITION('Reference_Motor_Envelope',
'Reference_Motor_Envelope',#40024,#40009);
#40017=PRODUCT_DEFINITION(
'hex bolt gradeab_iso_ISO 4014 - M4 x 25 x 14-N',
'hex bolt gradeab_iso_ISO 4014 - M4 x 25 x 14-N',#40025,#40009);
#40018=PRODUCT_DEFINITION_FORMATION('',$,#40037);
#40019=PRODUCT_DEFINITION_FORMATION('',$,#40038);
#40020=PRODUCT_DEFINITION_FORMATION('',$,#40039);
#40021=PRODUCT_DEFINITION_FORMATION('',$,#40040);
#40022=PRODUCT_DEFINITION_FORMATION('',$,#40041);
#40023=PRODUCT_DEFINITION_FORMATION('',$,#40042);
#40024=PRODUCT_DEFINITION_FORMATION('',$,#40043);
#40025=PRODUCT_DEFINITION_FORMATION('',$,#40044);
#40026=PRODUCT_RELATED_PRODUCT_CATEGORY(
'MAS-330','MAS-330',(#40037));
#40027=PRODUCT_RELATED_PRODUCT_CATEGORY('Main Cover','Main Cover',(#40038));
#40028=PRODUCT_RELATED_PRODUCT_CATEGORY('Central Rotor Drive Shaft',
'Central Rotor Drive Shaft',(#40039));
#40029=PRODUCT_RELATED_PRODUCT_CATEGORY('Flexible Tubing',
'Flexible Tubing',(#40040));
#40030=PRODUCT_RELATED_PRODUCT_CATEGORY('Motor Base','Motor Base',(#40041));
#40031=PRODUCT_RELATED_PRODUCT_CATEGORY('Cover with Sight Glass',
'Cover with Sight Glass',(#40042));
#40032=PRODUCT_RELATED_PRODUCT_CATEGORY('Reference_Motor_Envelope',
'Reference_Motor_Envelope',(#40043));
#40033=PRODUCT_RELATED_PRODUCT_CATEGORY(
'hex bolt gradeab_iso_ISO 4014 - M4 x 25 x 14-N',
'hex bolt gradeab_iso_ISO 4014 - M4 x 25 x 14-N',(#40044));
#40034=APPLICATION_PROTOCOL_DEFINITION('international standard',
'automotive_design',2009,#40035);
#40035=APPLICATION_CONTEXT(
'Core Data for Automotive Mechanical Design Process');
#40036=PRODUCT_CONTEXT('part definition',#40035,'mechanical');
#40037=PRODUCT('Flexible Tube Hose Pump',
'MAS-330','STEP AP214',(#40036));
#40038=PRODUCT('Main Cover','Main Cover',$,(#40036));
#40039=PRODUCT('Central Rotor Drive Shaft','Central Rotor Drive Shaft',
$,(#40036));
#40040=PRODUCT('Flexible Tubing','Flexible Tubing',$,(#40036));
#40041=PRODUCT('Motor Base','Motor Base',$,(#40036));
#40042=PRODUCT('Cover with Sight Glass','Cover with Sight Glass',$,(#40036));
#40043=PRODUCT('Reference_Motor_Envelope','Reference_Motor_Envelope',$,
(#40036));
#40044=PRODUCT('hex bolt gradeab_iso_ISO 4014 - M4 x 25 x 14-N',
'hex bolt gradeab_iso_ISO 4014 - M4 x 25 x 14-N',$,(#40036));
#40045=PRESENTATION_STYLE_ASSIGNMENT((#40047));
#40046=PRESENTATION_STYLE_ASSIGNMENT((#40048));
#40047=SURFACE_STYLE_USAGE(.BOTH.,#40049);
#40048=SURFACE_STYLE_USAGE(.BOTH.,#40050);
#40049=SURFACE_SIDE_STYLE('',(#40051));
#40050=SURFACE_SIDE_STYLE('',(#40052));
#40051=SURFACE_STYLE_FILL_AREA(#40053);
#40052=SURFACE_STYLE_FILL_AREA(#40054);
#40053=FILL_AREA_STYLE('Steel - Satin',(#40055));
#40054=FILL_AREA_STYLE('Opaque(202,209,238)',(#40056));
#40055=FILL_AREA_STYLE_COLOUR('Steel - Satin',#40057);
#40056=FILL_AREA_STYLE_COLOUR('Opaque(202,209,238)',#40058);
#40057=COLOUR_RGB('Steel - Satin', 0.09019608, 0.27058824, 0.51372549);
#40058=COLOUR_RGB('Opaque(202,209,238)', 0.66274510, 0.83137255, 0.94901961);
ENDSEC;
END-ISO-10303-21;
